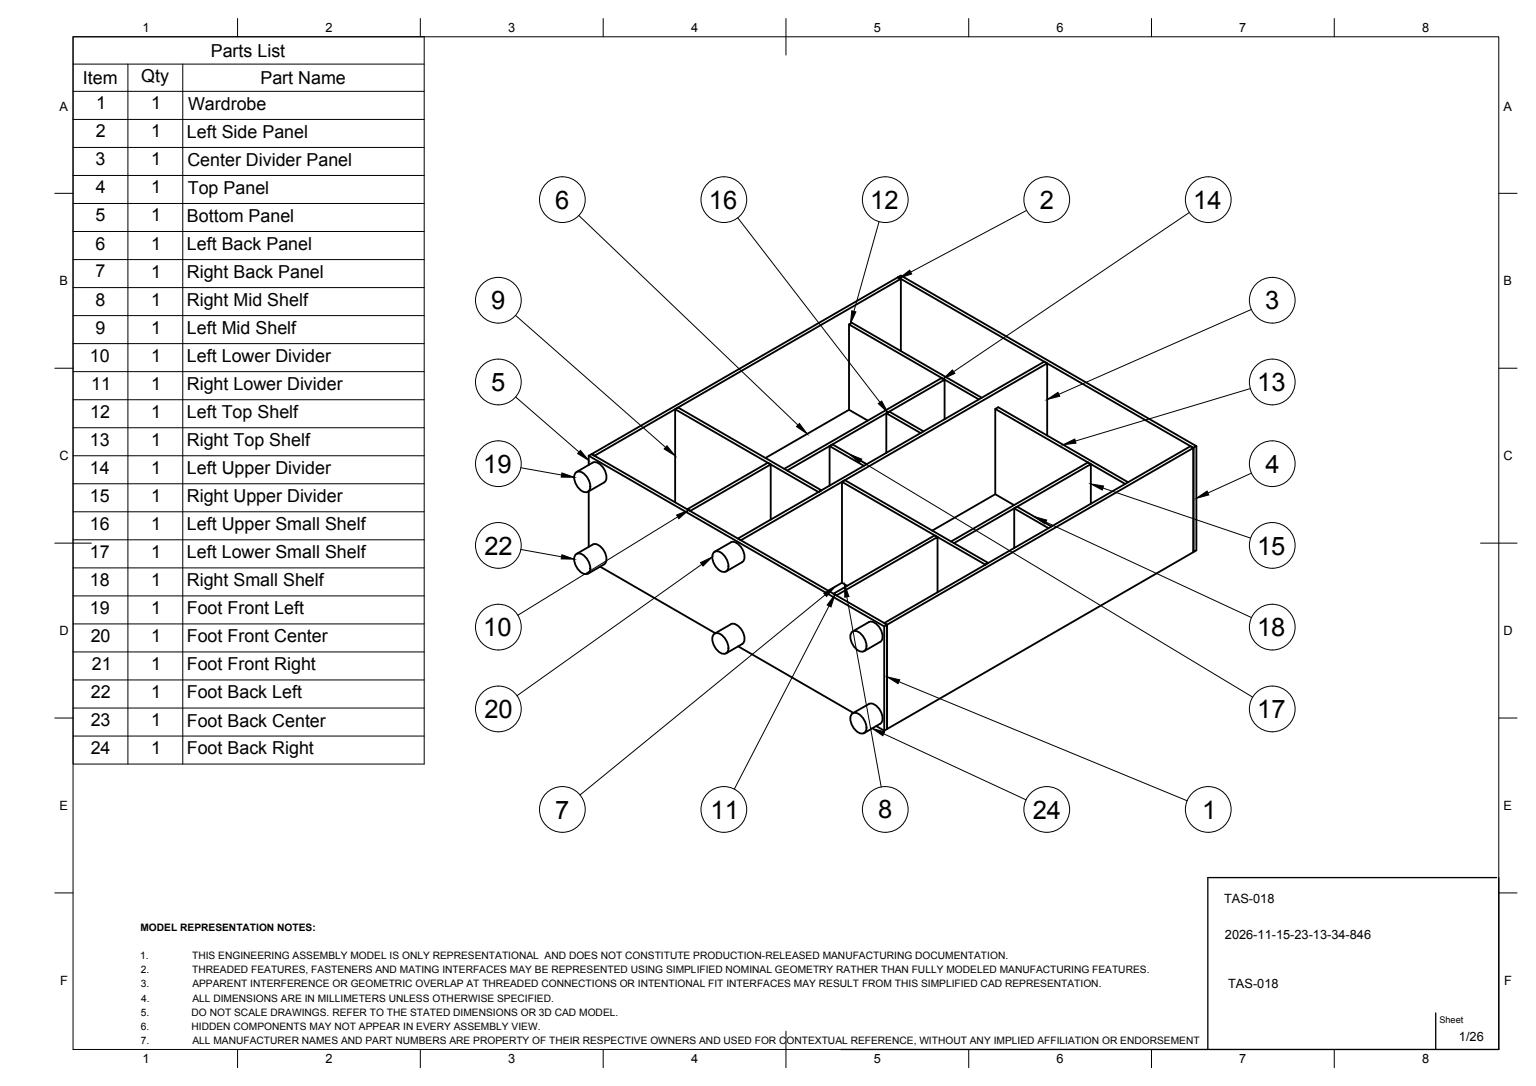
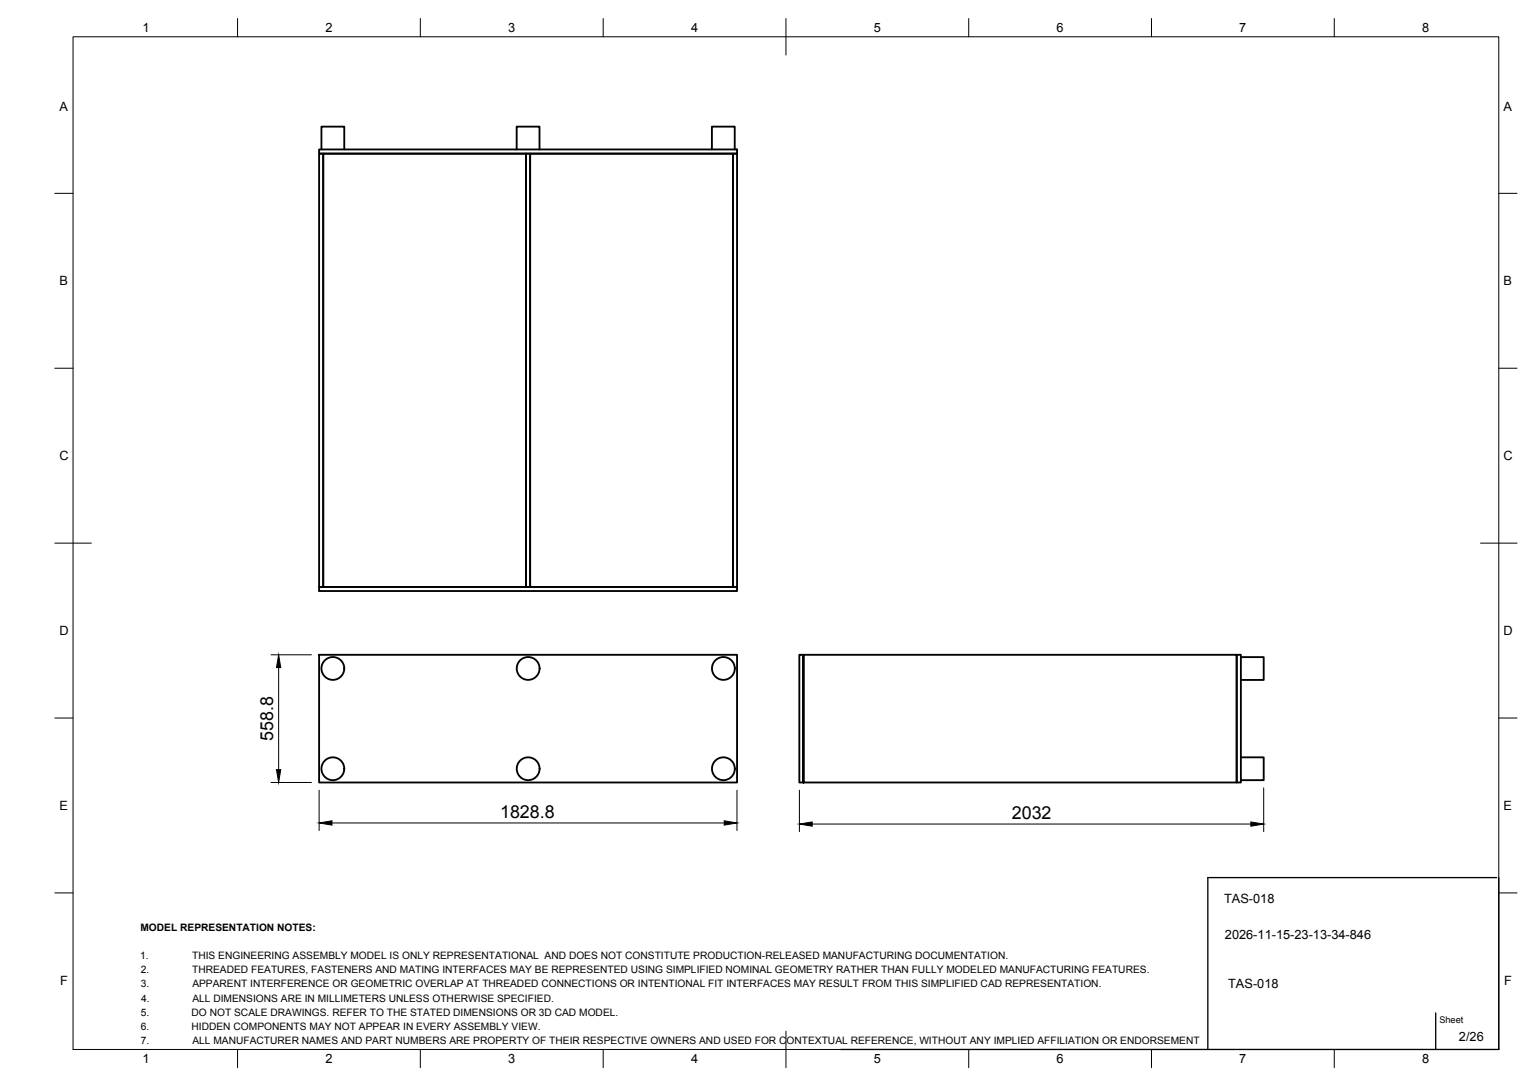
ISO-10303-21;
HEADER;
/* Generated by software containing ST-Developer
 * from STEP Tools, Inc. (www.steptools.com) 
 */

FILE_DESCRIPTION(
/* description */ (''),
/* implementation_level */ '2;1');

FILE_NAME(
/* name */ 'TAS-018.step',
/* time_stamp */ '2026-11-15T15:17:57-08:00',
/* author */ (''),
/* organization */ (''),
/* preprocessor_version */ 'ST-DEVELOPER v20.2',
/* originating_system */ 'Autodesk Translation Framework v15.17.0.0',
/* authorisation */ '');

FILE_SCHEMA (('AUTOMOTIVE_DESIGN { 1 0 10303 214 3 1 1 }'));
ENDSEC;

DATA;
#10=MECHANICAL_DESIGN_GEOMETRIC_PRESENTATION_REPRESENTATION('',(#177,#178,
#179,#180,#181,#182,#183,#184,#185,#186,#187,#188,#189,#190,#191,#192,#193,
#194,#195,#196,#197,#198,#199,#200),#3723);
#11=CIRCLE('',#2347,1.96850393700787);
#12=CIRCLE('',#2348,1.96850393700787);
#13=CIRCLE('',#2395,1.96850393700787);
#14=CIRCLE('',#2396,1.96850393700787);
#15=CIRCLE('',#2436,1.96850393700787);
#16=CIRCLE('',#2437,1.96850393700787);
#17=CIRCLE('',#2442,1.96850393700787);
#18=CIRCLE('',#2443,1.96850393700787);
#19=CIRCLE('',#2448,1.96850393700787);
#20=CIRCLE('',#2449,1.96850393700787);
#21=CIRCLE('',#2454,1.96850393700787);
#22=CIRCLE('',#2455,1.96850393700787);
#23=CYLINDRICAL_SURFACE('',#2346,1.96850393700787);
#24=CYLINDRICAL_SURFACE('',#2394,1.96850393700787);
#25=CYLINDRICAL_SURFACE('',#2435,1.96850393700787);
#26=CYLINDRICAL_SURFACE('',#2441,1.96850393700787);
#27=CYLINDRICAL_SURFACE('',#2447,1.96850393700787);
#28=CYLINDRICAL_SURFACE('',#2453,1.96850393700787);
#29=ITEM_DEFINED_TRANSFORMATION($,$,#2316,#2323);
#30=ITEM_DEFINED_TRANSFORMATION($,$,#2315,#2479);
#31=ITEM_DEFINED_TRANSFORMATION($,$,#2324,#2480);
#32=ITEM_DEFINED_TRANSFORMATION($,$,#2331,#2481);
#33=ITEM_DEFINED_TRANSFORMATION($,$,#2338,#2482);
#34=ITEM_DEFINED_TRANSFORMATION($,$,#2345,#2483);
#35=ITEM_DEFINED_TRANSFORMATION($,$,#2351,#2484);
#36=ITEM_DEFINED_TRANSFORMATION($,$,#2358,#2485);
#37=ITEM_DEFINED_TRANSFORMATION($,$,#2365,#2486);
#38=ITEM_DEFINED_TRANSFORMATION($,$,#2372,#2487);
#39=ITEM_DEFINED_TRANSFORMATION($,$,#2379,#2488);
#40=ITEM_DEFINED_TRANSFORMATION($,$,#2386,#2489);
#41=ITEM_DEFINED_TRANSFORMATION($,$,#2393,#2490);
#42=ITEM_DEFINED_TRANSFORMATION($,$,#2399,#2491);
#43=ITEM_DEFINED_TRANSFORMATION($,$,#2406,#2492);
#44=ITEM_DEFINED_TRANSFORMATION($,$,#2413,#2493);
#45=ITEM_DEFINED_TRANSFORMATION($,$,#2420,#2494);
#46=ITEM_DEFINED_TRANSFORMATION($,$,#2427,#2495);
#47=ITEM_DEFINED_TRANSFORMATION($,$,#2434,#2496);
#48=ITEM_DEFINED_TRANSFORMATION($,$,#2440,#2497);
#49=ITEM_DEFINED_TRANSFORMATION($,$,#2446,#2498);
#50=ITEM_DEFINED_TRANSFORMATION($,$,#2452,#2499);
#51=ITEM_DEFINED_TRANSFORMATION($,$,#2458,#2500);
#52=ITEM_DEFINED_TRANSFORMATION($,$,#2465,#2501);
#53=ITEM_DEFINED_TRANSFORMATION($,$,#2472,#2502);
#54=(
REPRESENTATION_RELATIONSHIP($,$,#3810,#3809)
REPRESENTATION_RELATIONSHIP_WITH_TRANSFORMATION(#29)
SHAPE_REPRESENTATION_RELATIONSHIP()
);
#55=(
REPRESENTATION_RELATIONSHIP($,$,#3809,#3808)
REPRESENTATION_RELATIONSHIP_WITH_TRANSFORMATION(#30)
SHAPE_REPRESENTATION_RELATIONSHIP()
);
#56=(
REPRESENTATION_RELATIONSHIP($,$,#3811,#3808)
REPRESENTATION_RELATIONSHIP_WITH_TRANSFORMATION(#31)
SHAPE_REPRESENTATION_RELATIONSHIP()
);
#57=(
REPRESENTATION_RELATIONSHIP($,$,#3812,#3808)
REPRESENTATION_RELATIONSHIP_WITH_TRANSFORMATION(#32)
SHAPE_REPRESENTATION_RELATIONSHIP()
);
#58=(
REPRESENTATION_RELATIONSHIP($,$,#3813,#3808)
REPRESENTATION_RELATIONSHIP_WITH_TRANSFORMATION(#33)
SHAPE_REPRESENTATION_RELATIONSHIP()
);
#59=(
REPRESENTATION_RELATIONSHIP($,$,#3814,#3808)
REPRESENTATION_RELATIONSHIP_WITH_TRANSFORMATION(#34)
SHAPE_REPRESENTATION_RELATIONSHIP()
);
#60=(
REPRESENTATION_RELATIONSHIP($,$,#3815,#3808)
REPRESENTATION_RELATIONSHIP_WITH_TRANSFORMATION(#35)
SHAPE_REPRESENTATION_RELATIONSHIP()
);
#61=(
REPRESENTATION_RELATIONSHIP($,$,#3816,#3808)
REPRESENTATION_RELATIONSHIP_WITH_TRANSFORMATION(#36)
SHAPE_REPRESENTATION_RELATIONSHIP()
);
#62=(
REPRESENTATION_RELATIONSHIP($,$,#3817,#3808)
REPRESENTATION_RELATIONSHIP_WITH_TRANSFORMATION(#37)
SHAPE_REPRESENTATION_RELATIONSHIP()
);
#63=(
REPRESENTATION_RELATIONSHIP($,$,#3818,#3808)
REPRESENTATION_RELATIONSHIP_WITH_TRANSFORMATION(#38)
SHAPE_REPRESENTATION_RELATIONSHIP()
);
#64=(
REPRESENTATION_RELATIONSHIP($,$,#3819,#3808)
REPRESENTATION_RELATIONSHIP_WITH_TRANSFORMATION(#39)
SHAPE_REPRESENTATION_RELATIONSHIP()
);
#65=(
REPRESENTATION_RELATIONSHIP($,$,#3820,#3808)
REPRESENTATION_RELATIONSHIP_WITH_TRANSFORMATION(#40)
SHAPE_REPRESENTATION_RELATIONSHIP()
);
#66=(
REPRESENTATION_RELATIONSHIP($,$,#3821,#3808)
REPRESENTATION_RELATIONSHIP_WITH_TRANSFORMATION(#41)
SHAPE_REPRESENTATION_RELATIONSHIP()
);
#67=(
REPRESENTATION_RELATIONSHIP($,$,#3822,#3808)
REPRESENTATION_RELATIONSHIP_WITH_TRANSFORMATION(#42)
SHAPE_REPRESENTATION_RELATIONSHIP()
);
#68=(
REPRESENTATION_RELATIONSHIP($,$,#3823,#3808)
REPRESENTATION_RELATIONSHIP_WITH_TRANSFORMATION(#43)
SHAPE_REPRESENTATION_RELATIONSHIP()
);
#69=(
REPRESENTATION_RELATIONSHIP($,$,#3824,#3808)
REPRESENTATION_RELATIONSHIP_WITH_TRANSFORMATION(#44)
SHAPE_REPRESENTATION_RELATIONSHIP()
);
#70=(
REPRESENTATION_RELATIONSHIP($,$,#3825,#3808)
REPRESENTATION_RELATIONSHIP_WITH_TRANSFORMATION(#45)
SHAPE_REPRESENTATION_RELATIONSHIP()
);
#71=(
REPRESENTATION_RELATIONSHIP($,$,#3826,#3808)
REPRESENTATION_RELATIONSHIP_WITH_TRANSFORMATION(#46)
SHAPE_REPRESENTATION_RELATIONSHIP()
);
#72=(
REPRESENTATION_RELATIONSHIP($,$,#3827,#3808)
REPRESENTATION_RELATIONSHIP_WITH_TRANSFORMATION(#47)
SHAPE_REPRESENTATION_RELATIONSHIP()
);
#73=(
REPRESENTATION_RELATIONSHIP($,$,#3828,#3808)
REPRESENTATION_RELATIONSHIP_WITH_TRANSFORMATION(#48)
SHAPE_REPRESENTATION_RELATIONSHIP()
);
#74=(
REPRESENTATION_RELATIONSHIP($,$,#3829,#3808)
REPRESENTATION_RELATIONSHIP_WITH_TRANSFORMATION(#49)
SHAPE_REPRESENTATION_RELATIONSHIP()
);
#75=(
REPRESENTATION_RELATIONSHIP($,$,#3830,#3808)
REPRESENTATION_RELATIONSHIP_WITH_TRANSFORMATION(#50)
SHAPE_REPRESENTATION_RELATIONSHIP()
);
#76=(
REPRESENTATION_RELATIONSHIP($,$,#3831,#3808)
REPRESENTATION_RELATIONSHIP_WITH_TRANSFORMATION(#51)
SHAPE_REPRESENTATION_RELATIONSHIP()
);
#77=(
REPRESENTATION_RELATIONSHIP($,$,#3832,#3808)
REPRESENTATION_RELATIONSHIP_WITH_TRANSFORMATION(#52)
SHAPE_REPRESENTATION_RELATIONSHIP()
);
#78=(
REPRESENTATION_RELATIONSHIP($,$,#3833,#3808)
REPRESENTATION_RELATIONSHIP_WITH_TRANSFORMATION(#53)
SHAPE_REPRESENTATION_RELATIONSHIP()
);
#79=CONTEXT_DEPENDENT_SHAPE_REPRESENTATION(#54,#3760);
#80=CONTEXT_DEPENDENT_SHAPE_REPRESENTATION(#55,#3784);
#81=CONTEXT_DEPENDENT_SHAPE_REPRESENTATION(#56,#3785);
#82=CONTEXT_DEPENDENT_SHAPE_REPRESENTATION(#57,#3786);
#83=CONTEXT_DEPENDENT_SHAPE_REPRESENTATION(#58,#3787);
#84=CONTEXT_DEPENDENT_SHAPE_REPRESENTATION(#59,#3788);
#85=CONTEXT_DEPENDENT_SHAPE_REPRESENTATION(#60,#3789);
#86=CONTEXT_DEPENDENT_SHAPE_REPRESENTATION(#61,#3790);
#87=CONTEXT_DEPENDENT_SHAPE_REPRESENTATION(#62,#3791);
#88=CONTEXT_DEPENDENT_SHAPE_REPRESENTATION(#63,#3792);
#89=CONTEXT_DEPENDENT_SHAPE_REPRESENTATION(#64,#3793);
#90=CONTEXT_DEPENDENT_SHAPE_REPRESENTATION(#65,#3794);
#91=CONTEXT_DEPENDENT_SHAPE_REPRESENTATION(#66,#3795);
#92=CONTEXT_DEPENDENT_SHAPE_REPRESENTATION(#67,#3796);
#93=CONTEXT_DEPENDENT_SHAPE_REPRESENTATION(#68,#3797);
#94=CONTEXT_DEPENDENT_SHAPE_REPRESENTATION(#69,#3798);
#95=CONTEXT_DEPENDENT_SHAPE_REPRESENTATION(#70,#3799);
#96=CONTEXT_DEPENDENT_SHAPE_REPRESENTATION(#71,#3800);
#97=CONTEXT_DEPENDENT_SHAPE_REPRESENTATION(#72,#3801);
#98=CONTEXT_DEPENDENT_SHAPE_REPRESENTATION(#73,#3802);
#99=CONTEXT_DEPENDENT_SHAPE_REPRESENTATION(#74,#3803);
#100=CONTEXT_DEPENDENT_SHAPE_REPRESENTATION(#75,#3804);
#101=CONTEXT_DEPENDENT_SHAPE_REPRESENTATION(#76,#3805);
#102=CONTEXT_DEPENDENT_SHAPE_REPRESENTATION(#77,#3806);
#103=CONTEXT_DEPENDENT_SHAPE_REPRESENTATION(#78,#3807);
#104=NEXT_ASSEMBLY_USAGE_OCCURRENCE('Right Side Panel:1',
'Right Side Panel:1','Right Side Panel:1',#3836,#3837,
'Right Side Panel:1');
#105=NEXT_ASSEMBLY_USAGE_OCCURRENCE('Wardrobe:1','Wardrobe:1',
'Wardrobe:1',#3835,#3836,'Wardrobe:1');
#106=NEXT_ASSEMBLY_USAGE_OCCURRENCE('Left Side Panel:1',
'Left Side Panel:1','Left Side Panel:1',#3835,#3838,'Left Side Panel:1');
#107=NEXT_ASSEMBLY_USAGE_OCCURRENCE('Center Divider Panel:1',
'Center Divider Panel:1','Center Divider Panel:1',#3835,#3839,
'Center Divider Panel:1');
#108=NEXT_ASSEMBLY_USAGE_OCCURRENCE('Left Lower Small Shelf:1',
'Left Lower Small Shelf:1','Left Lower Small Shelf:1',#3835,#3840,
'Left Lower Small Shelf:1');
#109=NEXT_ASSEMBLY_USAGE_OCCURRENCE('Foot Front Center:1',
'Foot Front Center:1','Foot Front Center:1',#3835,#3841,
'Foot Front Center:1');
#110=NEXT_ASSEMBLY_USAGE_OCCURRENCE('Left Lower Divider:1',
'Left Lower Divider:1','Left Lower Divider:1',#3835,#3842,
'Left Lower Divider:1');
#111=NEXT_ASSEMBLY_USAGE_OCCURRENCE('Right Top Shelf:1',
'Right Top Shelf:1','Right Top Shelf:1',#3835,#3843,'Right Top Shelf:1');
#112=NEXT_ASSEMBLY_USAGE_OCCURRENCE('Left Upper Small Shelf:1',
'Left Upper Small Shelf:1','Left Upper Small Shelf:1',#3835,#3844,
'Left Upper Small Shelf:1');
#113=NEXT_ASSEMBLY_USAGE_OCCURRENCE('Right Upper Divider:1',
'Right Upper Divider:1','Right Upper Divider:1',#3835,#3845,
'Right Upper Divider:1');
#114=NEXT_ASSEMBLY_USAGE_OCCURRENCE('Left Mid Shelf:1',
'Left Mid Shelf:1','Left Mid Shelf:1',#3835,#3846,'Left Mid Shelf:1');
#115=NEXT_ASSEMBLY_USAGE_OCCURRENCE('Right Lower Divider:1',
'Right Lower Divider:1','Right Lower Divider:1',#3835,#3847,
'Right Lower Divider:1');
#116=NEXT_ASSEMBLY_USAGE_OCCURRENCE('Foot Front Right:1',
'Foot Front Right:1','Foot Front Right:1',#3835,#3848,
'Foot Front Right:1');
#117=NEXT_ASSEMBLY_USAGE_OCCURRENCE('Right Mid Shelf:1',
'Right Mid Shelf:1','Right Mid Shelf:1',#3835,#3849,'Right Mid Shelf:1');
#118=NEXT_ASSEMBLY_USAGE_OCCURRENCE('Left Top Shelf:1',
'Left Top Shelf:1','Left Top Shelf:1',#3835,#3850,'Left Top Shelf:1');
#119=NEXT_ASSEMBLY_USAGE_OCCURRENCE('Right Small Shelf:1',
'Right Small Shelf:1','Right Small Shelf:1',#3835,#3851,
'Right Small Shelf:1');
#120=NEXT_ASSEMBLY_USAGE_OCCURRENCE('Left Upper Divider:1',
'Left Upper Divider:1','Left Upper Divider:1',#3835,#3852,
'Left Upper Divider:1');
#121=NEXT_ASSEMBLY_USAGE_OCCURRENCE('Top Panel:1','Top Panel:1',
'Top Panel:1',#3835,#3853,'Top Panel:1');
#122=NEXT_ASSEMBLY_USAGE_OCCURRENCE('Foot Front Left:1',
'Foot Front Left:1','Foot Front Left:1',#3835,#3854,'Foot Front Left:1');
#123=NEXT_ASSEMBLY_USAGE_OCCURRENCE('Foot Back Right:1',
'Foot Back Right:1','Foot Back Right:1',#3835,#3855,'Foot Back Right:1');
#124=NEXT_ASSEMBLY_USAGE_OCCURRENCE('Foot Back Left:1',
'Foot Back Left:1','Foot Back Left:1',#3835,#3856,'Foot Back Left:1');
#125=NEXT_ASSEMBLY_USAGE_OCCURRENCE('Foot Back Center:1',
'Foot Back Center:1','Foot Back Center:1',#3835,#3857,
'Foot Back Center:1');
#126=NEXT_ASSEMBLY_USAGE_OCCURRENCE('Left Back Panel:1',
'Left Back Panel:1','Left Back Panel:1',#3835,#3858,'Left Back Panel:1');
#127=NEXT_ASSEMBLY_USAGE_OCCURRENCE('Bottom Panel:1','Bottom Panel:1',
'Bottom Panel:1',#3835,#3859,'Bottom Panel:1');
#128=NEXT_ASSEMBLY_USAGE_OCCURRENCE('Right Back Panel:1',
'Right Back Panel:1','Right Back Panel:1',#3835,#3860,
'Right Back Panel:1');
#129=SHAPE_REPRESENTATION_RELATIONSHIP('SRR','None',#3810,#153);
#130=SHAPE_REPRESENTATION_RELATIONSHIP('SRR','None',#3811,#154);
#131=SHAPE_REPRESENTATION_RELATIONSHIP('SRR','None',#3812,#155);
#132=SHAPE_REPRESENTATION_RELATIONSHIP('SRR','None',#3813,#156);
#133=SHAPE_REPRESENTATION_RELATIONSHIP('SRR','None',#3814,#157);
#134=SHAPE_REPRESENTATION_RELATIONSHIP('SRR','None',#3815,#158);
#135=SHAPE_REPRESENTATION_RELATIONSHIP('SRR','None',#3816,#159);
#136=SHAPE_REPRESENTATION_RELATIONSHIP('SRR','None',#3817,#160);
#137=SHAPE_REPRESENTATION_RELATIONSHIP('SRR','None',#3818,#161);
#138=SHAPE_REPRESENTATION_RELATIONSHIP('SRR','None',#3819,#162);
#139=SHAPE_REPRESENTATION_RELATIONSHIP('SRR','None',#3820,#163);
#140=SHAPE_REPRESENTATION_RELATIONSHIP('SRR','None',#3821,#164);
#141=SHAPE_REPRESENTATION_RELATIONSHIP('SRR','None',#3822,#165);
#142=SHAPE_REPRESENTATION_RELATIONSHIP('SRR','None',#3823,#166);
#143=SHAPE_REPRESENTATION_RELATIONSHIP('SRR','None',#3824,#167);
#144=SHAPE_REPRESENTATION_RELATIONSHIP('SRR','None',#3825,#168);
#145=SHAPE_REPRESENTATION_RELATIONSHIP('SRR','None',#3826,#169);
#146=SHAPE_REPRESENTATION_RELATIONSHIP('SRR','None',#3827,#170);
#147=SHAPE_REPRESENTATION_RELATIONSHIP('SRR','None',#3828,#171);
#148=SHAPE_REPRESENTATION_RELATIONSHIP('SRR','None',#3829,#172);
#149=SHAPE_REPRESENTATION_RELATIONSHIP('SRR','None',#3830,#173);
#150=SHAPE_REPRESENTATION_RELATIONSHIP('SRR','None',#3831,#174);
#151=SHAPE_REPRESENTATION_RELATIONSHIP('SRR','None',#3832,#175);
#152=SHAPE_REPRESENTATION_RELATIONSHIP('SRR','None',#3833,#176);
#153=ADVANCED_BREP_SHAPE_REPRESENTATION('',(#201),#3699);
#154=ADVANCED_BREP_SHAPE_REPRESENTATION('',(#202),#3700);
#155=ADVANCED_BREP_SHAPE_REPRESENTATION('',(#203),#3701);
#156=ADVANCED_BREP_SHAPE_REPRESENTATION('',(#204),#3702);
#157=ADVANCED_BREP_SHAPE_REPRESENTATION('',(#205),#3703);
#158=ADVANCED_BREP_SHAPE_REPRESENTATION('',(#206),#3704);
#159=ADVANCED_BREP_SHAPE_REPRESENTATION('',(#207),#3705);
#160=ADVANCED_BREP_SHAPE_REPRESENTATION('',(#208),#3706);
#161=ADVANCED_BREP_SHAPE_REPRESENTATION('',(#209),#3707);
#162=ADVANCED_BREP_SHAPE_REPRESENTATION('',(#210),#3708);
#163=ADVANCED_BREP_SHAPE_REPRESENTATION('',(#211),#3709);
#164=ADVANCED_BREP_SHAPE_REPRESENTATION('',(#212),#3710);
#165=ADVANCED_BREP_SHAPE_REPRESENTATION('',(#213),#3711);
#166=ADVANCED_BREP_SHAPE_REPRESENTATION('',(#214),#3712);
#167=ADVANCED_BREP_SHAPE_REPRESENTATION('',(#215),#3713);
#168=ADVANCED_BREP_SHAPE_REPRESENTATION('',(#216),#3714);
#169=ADVANCED_BREP_SHAPE_REPRESENTATION('',(#217),#3715);
#170=ADVANCED_BREP_SHAPE_REPRESENTATION('',(#218),#3716);
#171=ADVANCED_BREP_SHAPE_REPRESENTATION('',(#219),#3717);
#172=ADVANCED_BREP_SHAPE_REPRESENTATION('',(#220),#3718);
#173=ADVANCED_BREP_SHAPE_REPRESENTATION('',(#221),#3719);
#174=ADVANCED_BREP_SHAPE_REPRESENTATION('',(#222),#3720);
#175=ADVANCED_BREP_SHAPE_REPRESENTATION('',(#223),#3721);
#176=ADVANCED_BREP_SHAPE_REPRESENTATION('',(#224),#3722);
#177=STYLED_ITEM('',(#3943),#201);
#178=STYLED_ITEM('',(#3943),#202);
#179=STYLED_ITEM('',(#3943),#203);
#180=STYLED_ITEM('',(#3944),#204);
#181=STYLED_ITEM('',(#3945),#205);
#182=STYLED_ITEM('',(#3946),#206);
#183=STYLED_ITEM('',(#3947),#207);
#184=STYLED_ITEM('',(#3944),#208);
#185=STYLED_ITEM('',(#3946),#209);
#186=STYLED_ITEM('',(#3947),#210);
#187=STYLED_ITEM('',(#3946),#211);
#188=STYLED_ITEM('',(#3945),#212);
#189=STYLED_ITEM('',(#3947),#213);
#190=STYLED_ITEM('',(#3947),#214);
#191=STYLED_ITEM('',(#3944),#215);
#192=STYLED_ITEM('',(#3946),#216);
#193=STYLED_ITEM('',(#3948),#217);
#194=STYLED_ITEM('',(#3945),#218);
#195=STYLED_ITEM('',(#3945),#219);
#196=STYLED_ITEM('',(#3945),#220);
#197=STYLED_ITEM('',(#3945),#221);
#198=STYLED_ITEM('',(#3949),#222);
#199=STYLED_ITEM('',(#3948),#223);
#200=STYLED_ITEM('',(#3949),#224);
#201=MANIFOLD_SOLID_BREP('Body1',#2025);
#202=MANIFOLD_SOLID_BREP('Body1',#2026);
#203=MANIFOLD_SOLID_BREP('Body1',#2027);
#204=MANIFOLD_SOLID_BREP('Body1',#2028);
#205=MANIFOLD_SOLID_BREP('Body1',#2029);
#206=MANIFOLD_SOLID_BREP('Body1',#2030);
#207=MANIFOLD_SOLID_BREP('Body1',#2031);
#208=MANIFOLD_SOLID_BREP('Body1',#2032);
#209=MANIFOLD_SOLID_BREP('Body1',#2033);
#210=MANIFOLD_SOLID_BREP('Body1',#2034);
#211=MANIFOLD_SOLID_BREP('Body1',#2035);
#212=MANIFOLD_SOLID_BREP('Body1',#2036);
#213=MANIFOLD_SOLID_BREP('Body1',#2037);
#214=MANIFOLD_SOLID_BREP('Body1',#2038);
#215=MANIFOLD_SOLID_BREP('Body1',#2039);
#216=MANIFOLD_SOLID_BREP('Body1',#2040);
#217=MANIFOLD_SOLID_BREP('Body1',#2041);
#218=MANIFOLD_SOLID_BREP('Body1',#2042);
#219=MANIFOLD_SOLID_BREP('Body1',#2043);
#220=MANIFOLD_SOLID_BREP('Body1',#2044);
#221=MANIFOLD_SOLID_BREP('Body1',#2045);
#222=MANIFOLD_SOLID_BREP('Body1',#2046);
#223=MANIFOLD_SOLID_BREP('Body1',#2047);
#224=MANIFOLD_SOLID_BREP('Body1',#2048);
#225=FACE_OUTER_BOUND('',#351,.T.);
#226=FACE_OUTER_BOUND('',#352,.T.);
#227=FACE_OUTER_BOUND('',#353,.T.);
#228=FACE_OUTER_BOUND('',#354,.T.);
#229=FACE_OUTER_BOUND('',#355,.T.);
#230=FACE_OUTER_BOUND('',#356,.T.);
#231=FACE_OUTER_BOUND('',#357,.T.);
#232=FACE_OUTER_BOUND('',#358,.T.);
#233=FACE_OUTER_BOUND('',#359,.T.);
#234=FACE_OUTER_BOUND('',#360,.T.);
#235=FACE_OUTER_BOUND('',#361,.T.);
#236=FACE_OUTER_BOUND('',#362,.T.);
#237=FACE_OUTER_BOUND('',#363,.T.);
#238=FACE_OUTER_BOUND('',#364,.T.);
#239=FACE_OUTER_BOUND('',#365,.T.);
#240=FACE_OUTER_BOUND('',#366,.T.);
#241=FACE_OUTER_BOUND('',#367,.T.);
#242=FACE_OUTER_BOUND('',#368,.T.);
#243=FACE_OUTER_BOUND('',#369,.T.);
#244=FACE_OUTER_BOUND('',#370,.T.);
#245=FACE_OUTER_BOUND('',#371,.T.);
#246=FACE_OUTER_BOUND('',#372,.T.);
#247=FACE_OUTER_BOUND('',#373,.T.);
#248=FACE_OUTER_BOUND('',#374,.T.);
#249=FACE_OUTER_BOUND('',#375,.T.);
#250=FACE_OUTER_BOUND('',#376,.T.);
#251=FACE_OUTER_BOUND('',#377,.T.);
#252=FACE_OUTER_BOUND('',#378,.T.);
#253=FACE_OUTER_BOUND('',#379,.T.);
#254=FACE_OUTER_BOUND('',#380,.T.);
#255=FACE_OUTER_BOUND('',#381,.T.);
#256=FACE_OUTER_BOUND('',#382,.T.);
#257=FACE_OUTER_BOUND('',#383,.T.);
#258=FACE_OUTER_BOUND('',#384,.T.);
#259=FACE_OUTER_BOUND('',#385,.T.);
#260=FACE_OUTER_BOUND('',#386,.T.);
#261=FACE_OUTER_BOUND('',#387,.T.);
#262=FACE_OUTER_BOUND('',#388,.T.);
#263=FACE_OUTER_BOUND('',#389,.T.);
#264=FACE_OUTER_BOUND('',#390,.T.);
#265=FACE_OUTER_BOUND('',#391,.T.);
#266=FACE_OUTER_BOUND('',#392,.T.);
#267=FACE_OUTER_BOUND('',#393,.T.);
#268=FACE_OUTER_BOUND('',#394,.T.);
#269=FACE_OUTER_BOUND('',#395,.T.);
#270=FACE_OUTER_BOUND('',#396,.T.);
#271=FACE_OUTER_BOUND('',#397,.T.);
#272=FACE_OUTER_BOUND('',#398,.T.);
#273=FACE_OUTER_BOUND('',#399,.T.);
#274=FACE_OUTER_BOUND('',#400,.T.);
#275=FACE_OUTER_BOUND('',#401,.T.);
#276=FACE_OUTER_BOUND('',#402,.T.);
#277=FACE_OUTER_BOUND('',#403,.T.);
#278=FACE_OUTER_BOUND('',#404,.T.);
#279=FACE_OUTER_BOUND('',#405,.T.);
#280=FACE_OUTER_BOUND('',#406,.T.);
#281=FACE_OUTER_BOUND('',#407,.T.);
#282=FACE_OUTER_BOUND('',#408,.T.);
#283=FACE_OUTER_BOUND('',#409,.T.);
#284=FACE_OUTER_BOUND('',#410,.T.);
#285=FACE_OUTER_BOUND('',#411,.T.);
#286=FACE_OUTER_BOUND('',#412,.T.);
#287=FACE_OUTER_BOUND('',#413,.T.);
#288=FACE_OUTER_BOUND('',#414,.T.);
#289=FACE_OUTER_BOUND('',#415,.T.);
#290=FACE_OUTER_BOUND('',#416,.T.);
#291=FACE_OUTER_BOUND('',#417,.T.);
#292=FACE_OUTER_BOUND('',#418,.T.);
#293=FACE_OUTER_BOUND('',#419,.T.);
#294=FACE_OUTER_BOUND('',#420,.T.);
#295=FACE_OUTER_BOUND('',#421,.T.);
#296=FACE_OUTER_BOUND('',#422,.T.);
#297=FACE_OUTER_BOUND('',#423,.T.);
#298=FACE_OUTER_BOUND('',#424,.T.);
#299=FACE_OUTER_BOUND('',#425,.T.);
#300=FACE_OUTER_BOUND('',#426,.T.);
#301=FACE_OUTER_BOUND('',#427,.T.);
#302=FACE_OUTER_BOUND('',#428,.T.);
#303=FACE_OUTER_BOUND('',#429,.T.);
#304=FACE_OUTER_BOUND('',#430,.T.);
#305=FACE_OUTER_BOUND('',#431,.T.);
#306=FACE_OUTER_BOUND('',#432,.T.);
#307=FACE_OUTER_BOUND('',#433,.T.);
#308=FACE_OUTER_BOUND('',#434,.T.);
#309=FACE_OUTER_BOUND('',#435,.T.);
#310=FACE_OUTER_BOUND('',#436,.T.);
#311=FACE_OUTER_BOUND('',#437,.T.);
#312=FACE_OUTER_BOUND('',#438,.T.);
#313=FACE_OUTER_BOUND('',#439,.T.);
#314=FACE_OUTER_BOUND('',#440,.T.);
#315=FACE_OUTER_BOUND('',#441,.T.);
#316=FACE_OUTER_BOUND('',#442,.T.);
#317=FACE_OUTER_BOUND('',#443,.T.);
#318=FACE_OUTER_BOUND('',#444,.T.);
#319=FACE_OUTER_BOUND('',#445,.T.);
#320=FACE_OUTER_BOUND('',#446,.T.);
#321=FACE_OUTER_BOUND('',#447,.T.);
#322=FACE_OUTER_BOUND('',#448,.T.);
#323=FACE_OUTER_BOUND('',#449,.T.);
#324=FACE_OUTER_BOUND('',#450,.T.);
#325=FACE_OUTER_BOUND('',#451,.T.);
#326=FACE_OUTER_BOUND('',#452,.T.);
#327=FACE_OUTER_BOUND('',#453,.T.);
#328=FACE_OUTER_BOUND('',#454,.T.);
#329=FACE_OUTER_BOUND('',#455,.T.);
#330=FACE_OUTER_BOUND('',#456,.T.);
#331=FACE_OUTER_BOUND('',#457,.T.);
#332=FACE_OUTER_BOUND('',#458,.T.);
#333=FACE_OUTER_BOUND('',#459,.T.);
#334=FACE_OUTER_BOUND('',#460,.T.);
#335=FACE_OUTER_BOUND('',#461,.T.);
#336=FACE_OUTER_BOUND('',#462,.T.);
#337=FACE_OUTER_BOUND('',#463,.T.);
#338=FACE_OUTER_BOUND('',#464,.T.);
#339=FACE_OUTER_BOUND('',#465,.T.);
#340=FACE_OUTER_BOUND('',#466,.T.);
#341=FACE_OUTER_BOUND('',#467,.T.);
#342=FACE_OUTER_BOUND('',#468,.T.);
#343=FACE_OUTER_BOUND('',#469,.T.);
#344=FACE_OUTER_BOUND('',#470,.T.);
#345=FACE_OUTER_BOUND('',#471,.T.);
#346=FACE_OUTER_BOUND('',#472,.T.);
#347=FACE_OUTER_BOUND('',#473,.T.);
#348=FACE_OUTER_BOUND('',#474,.T.);
#349=FACE_OUTER_BOUND('',#475,.T.);
#350=FACE_OUTER_BOUND('',#476,.T.);
#351=EDGE_LOOP('',(#1311,#1312,#1313,#1314));
#352=EDGE_LOOP('',(#1315,#1316,#1317,#1318));
#353=EDGE_LOOP('',(#1319,#1320,#1321,#1322));
#354=EDGE_LOOP('',(#1323,#1324,#1325,#1326));
#355=EDGE_LOOP('',(#1327,#1328,#1329,#1330));
#356=EDGE_LOOP('',(#1331,#1332,#1333,#1334));
#357=EDGE_LOOP('',(#1335,#1336,#1337,#1338));
#358=EDGE_LOOP('',(#1339,#1340,#1341,#1342));
#359=EDGE_LOOP('',(#1343,#1344,#1345,#1346));
#360=EDGE_LOOP('',(#1347,#1348,#1349,#1350));
#361=EDGE_LOOP('',(#1351,#1352,#1353,#1354));
#362=EDGE_LOOP('',(#1355,#1356,#1357,#1358));
#363=EDGE_LOOP('',(#1359,#1360,#1361,#1362));
#364=EDGE_LOOP('',(#1363,#1364,#1365,#1366));
#365=EDGE_LOOP('',(#1367,#1368,#1369,#1370));
#366=EDGE_LOOP('',(#1371,#1372,#1373,#1374));
#367=EDGE_LOOP('',(#1375,#1376,#1377,#1378));
#368=EDGE_LOOP('',(#1379,#1380,#1381,#1382));
#369=EDGE_LOOP('',(#1383,#1384,#1385,#1386));
#370=EDGE_LOOP('',(#1387,#1388,#1389,#1390));
#371=EDGE_LOOP('',(#1391,#1392,#1393,#1394));
#372=EDGE_LOOP('',(#1395,#1396,#1397,#1398));
#373=EDGE_LOOP('',(#1399,#1400,#1401,#1402));
#374=EDGE_LOOP('',(#1403,#1404,#1405,#1406));
#375=EDGE_LOOP('',(#1407,#1408,#1409,#1410));
#376=EDGE_LOOP('',(#1411));
#377=EDGE_LOOP('',(#1412));
#378=EDGE_LOOP('',(#1413,#1414,#1415,#1416));
#379=EDGE_LOOP('',(#1417,#1418,#1419,#1420));
#380=EDGE_LOOP('',(#1421,#1422,#1423,#1424));
#381=EDGE_LOOP('',(#1425,#1426,#1427,#1428));
#382=EDGE_LOOP('',(#1429,#1430,#1431,#1432));
#383=EDGE_LOOP('',(#1433,#1434,#1435,#1436));
#384=EDGE_LOOP('',(#1437,#1438,#1439,#1440));
#385=EDGE_LOOP('',(#1441,#1442,#1443,#1444));
#386=EDGE_LOOP('',(#1445,#1446,#1447,#1448));
#387=EDGE_LOOP('',(#1449,#1450,#1451,#1452));
#388=EDGE_LOOP('',(#1453,#1454,#1455,#1456));
#389=EDGE_LOOP('',(#1457,#1458,#1459,#1460));
#390=EDGE_LOOP('',(#1461,#1462,#1463,#1464));
#391=EDGE_LOOP('',(#1465,#1466,#1467,#1468));
#392=EDGE_LOOP('',(#1469,#1470,#1471,#1472));
#393=EDGE_LOOP('',(#1473,#1474,#1475,#1476));
#394=EDGE_LOOP('',(#1477,#1478,#1479,#1480));
#395=EDGE_LOOP('',(#1481,#1482,#1483,#1484));
#396=EDGE_LOOP('',(#1485,#1486,#1487,#1488));
#397=EDGE_LOOP('',(#1489,#1490,#1491,#1492));
#398=EDGE_LOOP('',(#1493,#1494,#1495,#1496));
#399=EDGE_LOOP('',(#1497,#1498,#1499,#1500));
#400=EDGE_LOOP('',(#1501,#1502,#1503,#1504));
#401=EDGE_LOOP('',(#1505,#1506,#1507,#1508));
#402=EDGE_LOOP('',(#1509,#1510,#1511,#1512));
#403=EDGE_LOOP('',(#1513,#1514,#1515,#1516));
#404=EDGE_LOOP('',(#1517,#1518,#1519,#1520));
#405=EDGE_LOOP('',(#1521,#1522,#1523,#1524));
#406=EDGE_LOOP('',(#1525,#1526,#1527,#1528));
#407=EDGE_LOOP('',(#1529,#1530,#1531,#1532));
#408=EDGE_LOOP('',(#1533,#1534,#1535,#1536));
#409=EDGE_LOOP('',(#1537,#1538,#1539,#1540));
#410=EDGE_LOOP('',(#1541,#1542,#1543,#1544));
#411=EDGE_LOOP('',(#1545,#1546,#1547,#1548));
#412=EDGE_LOOP('',(#1549,#1550,#1551,#1552));
#413=EDGE_LOOP('',(#1553,#1554,#1555,#1556));
#414=EDGE_LOOP('',(#1557,#1558,#1559,#1560));
#415=EDGE_LOOP('',(#1561));
#416=EDGE_LOOP('',(#1562));
#417=EDGE_LOOP('',(#1563,#1564,#1565,#1566));
#418=EDGE_LOOP('',(#1567,#1568,#1569,#1570));
#419=EDGE_LOOP('',(#1571,#1572,#1573,#1574));
#420=EDGE_LOOP('',(#1575,#1576,#1577,#1578));
#421=EDGE_LOOP('',(#1579,#1580,#1581,#1582));
#422=EDGE_LOOP('',(#1583,#1584,#1585,#1586));
#423=EDGE_LOOP('',(#1587,#1588,#1589,#1590));
#424=EDGE_LOOP('',(#1591,#1592,#1593,#1594));
#425=EDGE_LOOP('',(#1595,#1596,#1597,#1598));
#426=EDGE_LOOP('',(#1599,#1600,#1601,#1602));
#427=EDGE_LOOP('',(#1603,#1604,#1605,#1606));
#428=EDGE_LOOP('',(#1607,#1608,#1609,#1610));
#429=EDGE_LOOP('',(#1611,#1612,#1613,#1614));
#430=EDGE_LOOP('',(#1615,#1616,#1617,#1618));
#431=EDGE_LOOP('',(#1619,#1620,#1621,#1622));
#432=EDGE_LOOP('',(#1623,#1624,#1625,#1626));
#433=EDGE_LOOP('',(#1627,#1628,#1629,#1630));
#434=EDGE_LOOP('',(#1631,#1632,#1633,#1634));
#435=EDGE_LOOP('',(#1635,#1636,#1637,#1638));
#436=EDGE_LOOP('',(#1639,#1640,#1641,#1642));
#437=EDGE_LOOP('',(#1643,#1644,#1645,#1646));
#438=EDGE_LOOP('',(#1647,#1648,#1649,#1650));
#439=EDGE_LOOP('',(#1651,#1652,#1653,#1654));
#440=EDGE_LOOP('',(#1655,#1656,#1657,#1658));
#441=EDGE_LOOP('',(#1659,#1660,#1661,#1662));
#442=EDGE_LOOP('',(#1663,#1664,#1665,#1666));
#443=EDGE_LOOP('',(#1667,#1668,#1669,#1670));
#444=EDGE_LOOP('',(#1671,#1672,#1673,#1674));
#445=EDGE_LOOP('',(#1675,#1676,#1677,#1678));
#446=EDGE_LOOP('',(#1679,#1680,#1681,#1682));
#447=EDGE_LOOP('',(#1683,#1684,#1685,#1686));
#448=EDGE_LOOP('',(#1687));
#449=EDGE_LOOP('',(#1688));
#450=EDGE_LOOP('',(#1689,#1690,#1691,#1692));
#451=EDGE_LOOP('',(#1693));
#452=EDGE_LOOP('',(#1694));
#453=EDGE_LOOP('',(#1695,#1696,#1697,#1698));
#454=EDGE_LOOP('',(#1699));
#455=EDGE_LOOP('',(#1700));
#456=EDGE_LOOP('',(#1701,#1702,#1703,#1704));
#457=EDGE_LOOP('',(#1705));
#458=EDGE_LOOP('',(#1706));
#459=EDGE_LOOP('',(#1707,#1708,#1709,#1710));
#460=EDGE_LOOP('',(#1711,#1712,#1713,#1714));
#461=EDGE_LOOP('',(#1715,#1716,#1717,#1718));
#462=EDGE_LOOP('',(#1719,#1720,#1721,#1722));
#463=EDGE_LOOP('',(#1723,#1724,#1725,#1726));
#464=EDGE_LOOP('',(#1727,#1728,#1729,#1730));
#465=EDGE_LOOP('',(#1731,#1732,#1733,#1734));
#466=EDGE_LOOP('',(#1735,#1736,#1737,#1738));
#467=EDGE_LOOP('',(#1739,#1740,#1741,#1742));
#468=EDGE_LOOP('',(#1743,#1744,#1745,#1746));
#469=EDGE_LOOP('',(#1747,#1748,#1749,#1750));
#470=EDGE_LOOP('',(#1751,#1752,#1753,#1754));
#471=EDGE_LOOP('',(#1755,#1756,#1757,#1758));
#472=EDGE_LOOP('',(#1759,#1760,#1761,#1762));
#473=EDGE_LOOP('',(#1763,#1764,#1765,#1766));
#474=EDGE_LOOP('',(#1767,#1768,#1769,#1770));
#475=EDGE_LOOP('',(#1771,#1772,#1773,#1774));
#476=EDGE_LOOP('',(#1775,#1776,#1777,#1778));
#477=LINE('',#3109,#699);
#478=LINE('',#3111,#700);
#479=LINE('',#3113,#701);
#480=LINE('',#3114,#702);
#481=LINE('',#3117,#703);
#482=LINE('',#3119,#704);
#483=LINE('',#3120,#705);
#484=LINE('',#3123,#706);
#485=LINE('',#3125,#707);
#486=LINE('',#3126,#708);
#487=LINE('',#3128,#709);
#488=LINE('',#3129,#710);
#489=LINE('',#3137,#711);
#490=LINE('',#3139,#712);
#491=LINE('',#3141,#713);
#492=LINE('',#3142,#714);
#493=LINE('',#3145,#715);
#494=LINE('',#3147,#716);
#495=LINE('',#3148,#717);
#496=LINE('',#3151,#718);
#497=LINE('',#3153,#719);
#498=LINE('',#3154,#720);
#499=LINE('',#3156,#721);
#500=LINE('',#3157,#722);
#501=LINE('',#3164,#723);
#502=LINE('',#3166,#724);
#503=LINE('',#3168,#725);
#504=LINE('',#3169,#726);
#505=LINE('',#3172,#727);
#506=LINE('',#3174,#728);
#507=LINE('',#3175,#729);
#508=LINE('',#3178,#730);
#509=LINE('',#3180,#731);
#510=LINE('',#3181,#732);
#511=LINE('',#3183,#733);
#512=LINE('',#3184,#734);
#513=LINE('',#3191,#735);
#514=LINE('',#3193,#736);
#515=LINE('',#3195,#737);
#516=LINE('',#3196,#738);
#517=LINE('',#3199,#739);
#518=LINE('',#3201,#740);
#519=LINE('',#3202,#741);
#520=LINE('',#3205,#742);
#521=LINE('',#3207,#743);
#522=LINE('',#3208,#744);
#523=LINE('',#3210,#745);
#524=LINE('',#3211,#746);
#525=LINE('',#3219,#747);
#526=LINE('',#3227,#748);
#527=LINE('',#3229,#749);
#528=LINE('',#3231,#750);
#529=LINE('',#3232,#751);
#530=LINE('',#3235,#752);
#531=LINE('',#3237,#753);
#532=LINE('',#3238,#754);
#533=LINE('',#3241,#755);
#534=LINE('',#3243,#756);
#535=LINE('',#3244,#757);
#536=LINE('',#3246,#758);
#537=LINE('',#3247,#759);
#538=LINE('',#3254,#760);
#539=LINE('',#3256,#761);
#540=LINE('',#3258,#762);
#541=LINE('',#3259,#763);
#542=LINE('',#3262,#764);
#543=LINE('',#3264,#765);
#544=LINE('',#3265,#766);
#545=LINE('',#3268,#767);
#546=LINE('',#3270,#768);
#547=LINE('',#3271,#769);
#548=LINE('',#3273,#770);
#549=LINE('',#3274,#771);
#550=LINE('',#3281,#772);
#551=LINE('',#3283,#773);
#552=LINE('',#3285,#774);
#553=LINE('',#3286,#775);
#554=LINE('',#3289,#776);
#555=LINE('',#3291,#777);
#556=LINE('',#3292,#778);
#557=LINE('',#3295,#779);
#558=LINE('',#3297,#780);
#559=LINE('',#3298,#781);
#560=LINE('',#3300,#782);
#561=LINE('',#3301,#783);
#562=LINE('',#3308,#784);
#563=LINE('',#3310,#785);
#564=LINE('',#3312,#786);
#565=LINE('',#3313,#787);
#566=LINE('',#3316,#788);
#567=LINE('',#3318,#789);
#568=LINE('',#3319,#790);
#569=LINE('',#3322,#791);
#570=LINE('',#3324,#792);
#571=LINE('',#3325,#793);
#572=LINE('',#3327,#794);
#573=LINE('',#3328,#795);
#574=LINE('',#3335,#796);
#575=LINE('',#3337,#797);
#576=LINE('',#3339,#798);
#577=LINE('',#3340,#799);
#578=LINE('',#3344,#800);
#579=LINE('',#3346,#801);
#580=LINE('',#3348,#802);
#581=LINE('',#3349,#803);
#582=LINE('',#3351,#804);
#583=LINE('',#3352,#805);
#584=LINE('',#3354,#806);
#585=LINE('',#3356,#807);
#586=LINE('',#3362,#808);
#587=LINE('',#3364,#809);
#588=LINE('',#3366,#810);
#589=LINE('',#3367,#811);
#590=LINE('',#3371,#812);
#591=LINE('',#3372,#813);
#592=LINE('',#3373,#814);
#593=LINE('',#3376,#815);
#594=LINE('',#3378,#816);
#595=LINE('',#3379,#817);
#596=LINE('',#3381,#818);
#597=LINE('',#3382,#819);
#598=LINE('',#3390,#820);
#599=LINE('',#3398,#821);
#600=LINE('',#3400,#822);
#601=LINE('',#3402,#823);
#602=LINE('',#3403,#824);
#603=LINE('',#3407,#825);
#604=LINE('',#3409,#826);
#605=LINE('',#3411,#827);
#606=LINE('',#3412,#828);
#607=LINE('',#3414,#829);
#608=LINE('',#3415,#830);
#609=LINE('',#3417,#831);
#610=LINE('',#3419,#832);
#611=LINE('',#3425,#833);
#612=LINE('',#3427,#834);
#613=LINE('',#3429,#835);
#614=LINE('',#3430,#836);
#615=LINE('',#3433,#837);
#616=LINE('',#3435,#838);
#617=LINE('',#3436,#839);
#618=LINE('',#3439,#840);
#619=LINE('',#3441,#841);
#620=LINE('',#3442,#842);
#621=LINE('',#3444,#843);
#622=LINE('',#3445,#844);
#623=LINE('',#3452,#845);
#624=LINE('',#3454,#846);
#625=LINE('',#3456,#847);
#626=LINE('',#3457,#848);
#627=LINE('',#3460,#849);
#628=LINE('',#3462,#850);
#629=LINE('',#3463,#851);
#630=LINE('',#3466,#852);
#631=LINE('',#3468,#853);
#632=LINE('',#3469,#854);
#633=LINE('',#3471,#855);
#634=LINE('',#3472,#856);
#635=LINE('',#3479,#857);
#636=LINE('',#3481,#858);
#637=LINE('',#3483,#859);
#638=LINE('',#3484,#860);
#639=LINE('',#3487,#861);
#640=LINE('',#3489,#862);
#641=LINE('',#3490,#863);
#642=LINE('',#3493,#864);
#643=LINE('',#3495,#865);
#644=LINE('',#3496,#866);
#645=LINE('',#3498,#867);
#646=LINE('',#3499,#868);
#647=LINE('',#3506,#869);
#648=LINE('',#3508,#870);
#649=LINE('',#3510,#871);
#650=LINE('',#3511,#872);
#651=LINE('',#3514,#873);
#652=LINE('',#3516,#874);
#653=LINE('',#3517,#875);
#654=LINE('',#3520,#876);
#655=LINE('',#3522,#877);
#656=LINE('',#3523,#878);
#657=LINE('',#3525,#879);
#658=LINE('',#3526,#880);
#659=LINE('',#3534,#881);
#660=LINE('',#3543,#882);
#661=LINE('',#3552,#883);
#662=LINE('',#3561,#884);
#663=LINE('',#3569,#885);
#664=LINE('',#3571,#886);
#665=LINE('',#3573,#887);
#666=LINE('',#3574,#888);
#667=LINE('',#3577,#889);
#668=LINE('',#3579,#890);
#669=LINE('',#3580,#891);
#670=LINE('',#3583,#892);
#671=LINE('',#3585,#893);
#672=LINE('',#3586,#894);
#673=LINE('',#3588,#895);
#674=LINE('',#3589,#896);
#675=LINE('',#3596,#897);
#676=LINE('',#3598,#898);
#677=LINE('',#3600,#899);
#678=LINE('',#3601,#900);
#679=LINE('',#3604,#901);
#680=LINE('',#3606,#902);
#681=LINE('',#3607,#903);
#682=LINE('',#3610,#904);
#683=LINE('',#3612,#905);
#684=LINE('',#3613,#906);
#685=LINE('',#3615,#907);
#686=LINE('',#3616,#908);
#687=LINE('',#3623,#909);
#688=LINE('',#3625,#910);
#689=LINE('',#3627,#911);
#690=LINE('',#3628,#912);
#691=LINE('',#3631,#913);
#692=LINE('',#3633,#914);
#693=LINE('',#3634,#915);
#694=LINE('',#3637,#916);
#695=LINE('',#3639,#917);
#696=LINE('',#3640,#918);
#697=LINE('',#3642,#919);
#698=LINE('',#3643,#920);
#699=VECTOR('',#2511,74.6456692913386);
#700=VECTOR('',#2512,22.);
#701=VECTOR('',#2513,74.6456692913386);
#702=VECTOR('',#2514,22.);
#703=VECTOR('',#2517,0.708661417322833);
#704=VECTOR('',#2518,22.);
#705=VECTOR('',#2519,0.708661417322833);
#706=VECTOR('',#2522,74.6456692913386);
#707=VECTOR('',#2523,22.);
#708=VECTOR('',#2524,74.6456692913386);
#709=VECTOR('',#2527,0.708661417322833);
#710=VECTOR('',#2528,0.708661417322833);
#711=VECTOR('',#2539,74.6456692913386);
#712=VECTOR('',#2540,22.);
#713=VECTOR('',#2541,74.6456692913386);
#714=VECTOR('',#2542,22.);
#715=VECTOR('',#2545,0.708661417322833);
#716=VECTOR('',#2546,22.);
#717=VECTOR('',#2547,0.708661417322833);
#718=VECTOR('',#2550,74.6456692913386);
#719=VECTOR('',#2551,22.);
#720=VECTOR('',#2552,74.6456692913386);
#721=VECTOR('',#2555,0.708661417322833);
#722=VECTOR('',#2556,0.708661417322833);
#723=VECTOR('',#2565,74.6456692913386);
#724=VECTOR('',#2566,22.);
#725=VECTOR('',#2567,74.6456692913386);
#726=VECTOR('',#2568,22.);
#727=VECTOR('',#2571,0.708661417322835);
#728=VECTOR('',#2572,22.);
#729=VECTOR('',#2573,0.708661417322835);
#730=VECTOR('',#2576,74.6456692913386);
#731=VECTOR('',#2577,22.);
#732=VECTOR('',#2578,74.6456692913386);
#733=VECTOR('',#2581,0.708661417322835);
#734=VECTOR('',#2582,0.708661417322835);
#735=VECTOR('',#2591,0.708661417322833);
#736=VECTOR('',#2592,18.);
#737=VECTOR('',#2593,0.708661417322833);
#738=VECTOR('',#2594,18.);
#739=VECTOR('',#2597,11.6456692913385);
#740=VECTOR('',#2598,11.6456692913385);
#741=VECTOR('',#2599,18.);
#742=VECTOR('',#2602,0.708661417322833);
#743=VECTOR('',#2603,0.708661417322833);
#744=VECTOR('',#2604,18.);
#745=VECTOR('',#2607,11.6456692913385);
#746=VECTOR('',#2608,11.6456692913385);
#747=VECTOR('',#2619,1.96850393700787);
#748=VECTOR('',#2630,21.2913385826772);
#749=VECTOR('',#2631,19.6456692913386);
#750=VECTOR('',#2632,21.2913385826772);
#751=VECTOR('',#2633,19.6456692913386);
#752=VECTOR('',#2636,0.708661417322832);
#753=VECTOR('',#2637,0.708661417322832);
#754=VECTOR('',#2638,21.2913385826772);
#755=VECTOR('',#2641,19.6456692913386);
#756=VECTOR('',#2642,19.6456692913386);
#757=VECTOR('',#2643,21.2913385826772);
#758=VECTOR('',#2646,0.708661417322832);
#759=VECTOR('',#2647,0.708661417322832);
#760=VECTOR('',#2656,0.708661417322839);
#761=VECTOR('',#2657,18.);
#762=VECTOR('',#2658,0.708661417322839);
#763=VECTOR('',#2659,18.);
#764=VECTOR('',#2662,34.9370078740157);
#765=VECTOR('',#2663,18.);
#766=VECTOR('',#2664,34.9370078740157);
#767=VECTOR('',#2667,0.708661417322839);
#768=VECTOR('',#2668,18.);
#769=VECTOR('',#2669,0.708661417322839);
#770=VECTOR('',#2672,34.9370078740157);
#771=VECTOR('',#2673,34.9370078740157);
#772=VECTOR('',#2682,0.708661417322828);
#773=VECTOR('',#2683,18.);
#774=VECTOR('',#2684,0.708661417322828);
#775=VECTOR('',#2685,18.);
#776=VECTOR('',#2688,11.6456692913386);
#777=VECTOR('',#2689,11.6456692913386);
#778=VECTOR('',#2690,18.);
#779=VECTOR('',#2693,0.708661417322839);
#780=VECTOR('',#2694,0.708661417322839);
#781=VECTOR('',#2695,18.);
#782=VECTOR('',#2698,11.6456692913386);
#783=VECTOR('',#2699,11.6456692913386);
#784=VECTOR('',#2708,36.6456692913386);
#785=VECTOR('',#2709,18.);
#786=VECTOR('',#2710,36.6456692913386);
#787=VECTOR('',#2711,18.);
#788=VECTOR('',#2714,0.708661417322839);
#789=VECTOR('',#2715,0.708661417322839);
#790=VECTOR('',#2716,18.);
#791=VECTOR('',#2719,36.6456692913386);
#792=VECTOR('',#2720,36.6456692913386);
#793=VECTOR('',#2721,18.);
#794=VECTOR('',#2724,0.708661417322839);
#795=VECTOR('',#2725,0.708661417322839);
#796=VECTOR('',#2734,34.9370078740157);
#797=VECTOR('',#2735,0.708661417322831);
#798=VECTOR('',#2736,34.9370078740157);
#799=VECTOR('',#2737,0.708661417322831);
#800=VECTOR('',#2740,0.708661417322831);
#801=VECTOR('',#2741,34.9370078740157);
#802=VECTOR('',#2742,0.708661417322831);
#803=VECTOR('',#2743,34.9370078740157);
#804=VECTOR('',#2746,21.2913385826772);
#805=VECTOR('',#2747,21.2913385826772);
#806=VECTOR('',#2750,21.2913385826772);
#807=VECTOR('',#2753,21.2913385826772);
#808=VECTOR('',#2760,21.2913385826772);
#809=VECTOR('',#2761,24.6456692913386);
#810=VECTOR('',#2762,21.2913385826772);
#811=VECTOR('',#2763,24.6456692913386);
#812=VECTOR('',#2766,21.2913385826772);
#813=VECTOR('',#2767,0.708661417322836);
#814=VECTOR('',#2768,0.708661417322836);
#815=VECTOR('',#2771,24.6456692913386);
#816=VECTOR('',#2772,24.6456692913386);
#817=VECTOR('',#2773,21.2913385826772);
#818=VECTOR('',#2776,0.708661417322836);
#819=VECTOR('',#2777,0.708661417322836);
#820=VECTOR('',#2788,1.96850393700787);
#821=VECTOR('',#2799,34.9370078740157);
#822=VECTOR('',#2800,0.708661417322833);
#823=VECTOR('',#2801,34.9370078740157);
#824=VECTOR('',#2802,0.708661417322833);
#825=VECTOR('',#2805,0.708661417322833);
#826=VECTOR('',#2806,34.9370078740157);
#827=VECTOR('',#2807,0.708661417322833);
#828=VECTOR('',#2808,34.9370078740157);
#829=VECTOR('',#2811,21.2913385826772);
#830=VECTOR('',#2812,21.2913385826772);
#831=VECTOR('',#2815,21.2913385826772);
#832=VECTOR('',#2818,21.2913385826772);
#833=VECTOR('',#2825,0.708661417322839);
#834=VECTOR('',#2826,18.);
#835=VECTOR('',#2827,0.708661417322839);
#836=VECTOR('',#2828,18.);
#837=VECTOR('',#2831,34.9370078740157);
#838=VECTOR('',#2832,18.);
#839=VECTOR('',#2833,34.9370078740157);
#840=VECTOR('',#2836,0.708661417322839);
#841=VECTOR('',#2837,18.);
#842=VECTOR('',#2838,0.708661417322839);
#843=VECTOR('',#2841,34.9370078740157);
#844=VECTOR('',#2842,34.9370078740157);
#845=VECTOR('',#2851,0.708661417322833);
#846=VECTOR('',#2852,18.);
#847=VECTOR('',#2853,0.708661417322833);
#848=VECTOR('',#2854,18.);
#849=VECTOR('',#2857,11.6456692913386);
#850=VECTOR('',#2858,11.6456692913386);
#851=VECTOR('',#2859,18.);
#852=VECTOR('',#2862,0.708661417322845);
#853=VECTOR('',#2863,0.708661417322845);
#854=VECTOR('',#2864,18.);
#855=VECTOR('',#2867,11.6456692913386);
#856=VECTOR('',#2868,11.6456692913386);
#857=VECTOR('',#2877,41.6456692913386);
#858=VECTOR('',#2878,18.);
#859=VECTOR('',#2879,41.6456692913386);
#860=VECTOR('',#2880,18.);
#861=VECTOR('',#2883,0.708661417322838);
#862=VECTOR('',#2884,0.708661417322838);
#863=VECTOR('',#2885,18.);
#864=VECTOR('',#2888,41.6456692913386);
#865=VECTOR('',#2889,41.6456692913386);
#866=VECTOR('',#2890,18.);
#867=VECTOR('',#2893,0.708661417322836);
#868=VECTOR('',#2894,0.708661417322836);
#869=VECTOR('',#2903,22.);
#870=VECTOR('',#2904,0.708661417322828);
#871=VECTOR('',#2905,22.);
#872=VECTOR('',#2906,0.708661417322828);
#873=VECTOR('',#2909,72.);
#874=VECTOR('',#2910,0.708661417322828);
#875=VECTOR('',#2911,72.);
#876=VECTOR('',#2914,22.);
#877=VECTOR('',#2915,0.708661417322828);
#878=VECTOR('',#2916,22.);
#879=VECTOR('',#2919,72.);
#880=VECTOR('',#2920,72.);
#881=VECTOR('',#2931,1.96850393700787);
#882=VECTOR('',#2944,1.96850393700787);
#883=VECTOR('',#2957,1.96850393700787);
#884=VECTOR('',#2970,1.96850393700787);
#885=VECTOR('',#2981,74.6456692913386);
#886=VECTOR('',#2982,0.708661417322834);
#887=VECTOR('',#2983,74.6456692913386);
#888=VECTOR('',#2984,0.708661417322834);
#889=VECTOR('',#2987,34.9370078740157);
#890=VECTOR('',#2988,0.708661417322834);
#891=VECTOR('',#2989,34.9370078740157);
#892=VECTOR('',#2992,74.6456692913386);
#893=VECTOR('',#2993,0.708661417322834);
#894=VECTOR('',#2994,74.6456692913386);
#895=VECTOR('',#2997,34.9370078740157);
#896=VECTOR('',#2998,34.9370078740157);
#897=VECTOR('',#3007,22.);
#898=VECTOR('',#3008,0.708661417322835);
#899=VECTOR('',#3009,22.);
#900=VECTOR('',#3010,0.708661417322835);
#901=VECTOR('',#3013,72.);
#902=VECTOR('',#3014,0.708661417322835);
#903=VECTOR('',#3015,72.);
#904=VECTOR('',#3018,22.);
#905=VECTOR('',#3019,0.708661417322835);
#906=VECTOR('',#3020,22.);
#907=VECTOR('',#3023,72.);
#908=VECTOR('',#3024,72.);
#909=VECTOR('',#3033,74.6456692913386);
#910=VECTOR('',#3034,0.708661417322834);
#911=VECTOR('',#3035,74.6456692913386);
#912=VECTOR('',#3036,0.708661417322834);
#913=VECTOR('',#3039,34.9370078740157);
#914=VECTOR('',#3040,0.708661417322834);
#915=VECTOR('',#3041,34.9370078740157);
#916=VECTOR('',#3044,74.6456692913386);
#917=VECTOR('',#3045,0.708661417322834);
#918=VECTOR('',#3046,74.6456692913386);
#919=VECTOR('',#3049,34.9370078740157);
#920=VECTOR('',#3050,34.9370078740157);
#921=VERTEX_POINT('',#3107);
#922=VERTEX_POINT('',#3108);
#923=VERTEX_POINT('',#3110);
#924=VERTEX_POINT('',#3112);
#925=VERTEX_POINT('',#3116);
#926=VERTEX_POINT('',#3118);
#927=VERTEX_POINT('',#3122);
#928=VERTEX_POINT('',#3124);
#929=VERTEX_POINT('',#3135);
#930=VERTEX_POINT('',#3136);
#931=VERTEX_POINT('',#3138);
#932=VERTEX_POINT('',#3140);
#933=VERTEX_POINT('',#3144);
#934=VERTEX_POINT('',#3146);
#935=VERTEX_POINT('',#3150);
#936=VERTEX_POINT('',#3152);
#937=VERTEX_POINT('',#3162);
#938=VERTEX_POINT('',#3163);
#939=VERTEX_POINT('',#3165);
#940=VERTEX_POINT('',#3167);
#941=VERTEX_POINT('',#3171);
#942=VERTEX_POINT('',#3173);
#943=VERTEX_POINT('',#3177);
#944=VERTEX_POINT('',#3179);
#945=VERTEX_POINT('',#3189);
#946=VERTEX_POINT('',#3190);
#947=VERTEX_POINT('',#3192);
#948=VERTEX_POINT('',#3194);
#949=VERTEX_POINT('',#3198);
#950=VERTEX_POINT('',#3200);
#951=VERTEX_POINT('',#3204);
#952=VERTEX_POINT('',#3206);
#953=VERTEX_POINT('',#3216);
#954=VERTEX_POINT('',#3218);
#955=VERTEX_POINT('',#3225);
#956=VERTEX_POINT('',#3226);
#957=VERTEX_POINT('',#3228);
#958=VERTEX_POINT('',#3230);
#959=VERTEX_POINT('',#3234);
#960=VERTEX_POINT('',#3236);
#961=VERTEX_POINT('',#3240);
#962=VERTEX_POINT('',#3242);
#963=VERTEX_POINT('',#3252);
#964=VERTEX_POINT('',#3253);
#965=VERTEX_POINT('',#3255);
#966=VERTEX_POINT('',#3257);
#967=VERTEX_POINT('',#3261);
#968=VERTEX_POINT('',#3263);
#969=VERTEX_POINT('',#3267);
#970=VERTEX_POINT('',#3269);
#971=VERTEX_POINT('',#3279);
#972=VERTEX_POINT('',#3280);
#973=VERTEX_POINT('',#3282);
#974=VERTEX_POINT('',#3284);
#975=VERTEX_POINT('',#3288);
#976=VERTEX_POINT('',#3290);
#977=VERTEX_POINT('',#3294);
#978=VERTEX_POINT('',#3296);
#979=VERTEX_POINT('',#3306);
#980=VERTEX_POINT('',#3307);
#981=VERTEX_POINT('',#3309);
#982=VERTEX_POINT('',#3311);
#983=VERTEX_POINT('',#3315);
#984=VERTEX_POINT('',#3317);
#985=VERTEX_POINT('',#3321);
#986=VERTEX_POINT('',#3323);
#987=VERTEX_POINT('',#3333);
#988=VERTEX_POINT('',#3334);
#989=VERTEX_POINT('',#3336);
#990=VERTEX_POINT('',#3338);
#991=VERTEX_POINT('',#3342);
#992=VERTEX_POINT('',#3343);
#993=VERTEX_POINT('',#3345);
#994=VERTEX_POINT('',#3347);
#995=VERTEX_POINT('',#3360);
#996=VERTEX_POINT('',#3361);
#997=VERTEX_POINT('',#3363);
#998=VERTEX_POINT('',#3365);
#999=VERTEX_POINT('',#3369);
#1000=VERTEX_POINT('',#3370);
#1001=VERTEX_POINT('',#3375);
#1002=VERTEX_POINT('',#3377);
#1003=VERTEX_POINT('',#3387);
#1004=VERTEX_POINT('',#3389);
#1005=VERTEX_POINT('',#3396);
#1006=VERTEX_POINT('',#3397);
#1007=VERTEX_POINT('',#3399);
#1008=VERTEX_POINT('',#3401);
#1009=VERTEX_POINT('',#3405);
#1010=VERTEX_POINT('',#3406);
#1011=VERTEX_POINT('',#3408);
#1012=VERTEX_POINT('',#3410);
#1013=VERTEX_POINT('',#3423);
#1014=VERTEX_POINT('',#3424);
#1015=VERTEX_POINT('',#3426);
#1016=VERTEX_POINT('',#3428);
#1017=VERTEX_POINT('',#3432);
#1018=VERTEX_POINT('',#3434);
#1019=VERTEX_POINT('',#3438);
#1020=VERTEX_POINT('',#3440);
#1021=VERTEX_POINT('',#3450);
#1022=VERTEX_POINT('',#3451);
#1023=VERTEX_POINT('',#3453);
#1024=VERTEX_POINT('',#3455);
#1025=VERTEX_POINT('',#3459);
#1026=VERTEX_POINT('',#3461);
#1027=VERTEX_POINT('',#3465);
#1028=VERTEX_POINT('',#3467);
#1029=VERTEX_POINT('',#3477);
#1030=VERTEX_POINT('',#3478);
#1031=VERTEX_POINT('',#3480);
#1032=VERTEX_POINT('',#3482);
#1033=VERTEX_POINT('',#3486);
#1034=VERTEX_POINT('',#3488);
#1035=VERTEX_POINT('',#3492);
#1036=VERTEX_POINT('',#3494);
#1037=VERTEX_POINT('',#3504);
#1038=VERTEX_POINT('',#3505);
#1039=VERTEX_POINT('',#3507);
#1040=VERTEX_POINT('',#3509);
#1041=VERTEX_POINT('',#3513);
#1042=VERTEX_POINT('',#3515);
#1043=VERTEX_POINT('',#3519);
#1044=VERTEX_POINT('',#3521);
#1045=VERTEX_POINT('',#3531);
#1046=VERTEX_POINT('',#3533);
#1047=VERTEX_POINT('',#3540);
#1048=VERTEX_POINT('',#3542);
#1049=VERTEX_POINT('',#3549);
#1050=VERTEX_POINT('',#3551);
#1051=VERTEX_POINT('',#3558);
#1052=VERTEX_POINT('',#3560);
#1053=VERTEX_POINT('',#3567);
#1054=VERTEX_POINT('',#3568);
#1055=VERTEX_POINT('',#3570);
#1056=VERTEX_POINT('',#3572);
#1057=VERTEX_POINT('',#3576);
#1058=VERTEX_POINT('',#3578);
#1059=VERTEX_POINT('',#3582);
#1060=VERTEX_POINT('',#3584);
#1061=VERTEX_POINT('',#3594);
#1062=VERTEX_POINT('',#3595);
#1063=VERTEX_POINT('',#3597);
#1064=VERTEX_POINT('',#3599);
#1065=VERTEX_POINT('',#3603);
#1066=VERTEX_POINT('',#3605);
#1067=VERTEX_POINT('',#3609);
#1068=VERTEX_POINT('',#3611);
#1069=VERTEX_POINT('',#3621);
#1070=VERTEX_POINT('',#3622);
#1071=VERTEX_POINT('',#3624);
#1072=VERTEX_POINT('',#3626);
#1073=VERTEX_POINT('',#3630);
#1074=VERTEX_POINT('',#3632);
#1075=VERTEX_POINT('',#3636);
#1076=VERTEX_POINT('',#3638);
#1077=EDGE_CURVE('',#921,#922,#477,.T.);
#1078=EDGE_CURVE('',#923,#922,#478,.T.);
#1079=EDGE_CURVE('',#924,#923,#479,.T.);
#1080=EDGE_CURVE('',#924,#921,#480,.T.);
#1081=EDGE_CURVE('',#922,#925,#481,.T.);
#1082=EDGE_CURVE('',#926,#925,#482,.T.);
#1083=EDGE_CURVE('',#923,#926,#483,.T.);
#1084=EDGE_CURVE('',#925,#927,#484,.T.);
#1085=EDGE_CURVE('',#928,#927,#485,.T.);
#1086=EDGE_CURVE('',#926,#928,#486,.T.);
#1087=EDGE_CURVE('',#927,#921,#487,.T.);
#1088=EDGE_CURVE('',#928,#924,#488,.T.);
#1089=EDGE_CURVE('',#929,#930,#489,.T.);
#1090=EDGE_CURVE('',#931,#930,#490,.T.);
#1091=EDGE_CURVE('',#932,#931,#491,.T.);
#1092=EDGE_CURVE('',#932,#929,#492,.T.);
#1093=EDGE_CURVE('',#930,#933,#493,.T.);
#1094=EDGE_CURVE('',#934,#933,#494,.T.);
#1095=EDGE_CURVE('',#931,#934,#495,.T.);
#1096=EDGE_CURVE('',#933,#935,#496,.T.);
#1097=EDGE_CURVE('',#936,#935,#497,.T.);
#1098=EDGE_CURVE('',#934,#936,#498,.T.);
#1099=EDGE_CURVE('',#935,#929,#499,.T.);
#1100=EDGE_CURVE('',#936,#932,#500,.T.);
#1101=EDGE_CURVE('',#937,#938,#501,.T.);
#1102=EDGE_CURVE('',#939,#938,#502,.T.);
#1103=EDGE_CURVE('',#940,#939,#503,.T.);
#1104=EDGE_CURVE('',#940,#937,#504,.T.);
#1105=EDGE_CURVE('',#938,#941,#505,.T.);
#1106=EDGE_CURVE('',#942,#941,#506,.T.);
#1107=EDGE_CURVE('',#939,#942,#507,.T.);
#1108=EDGE_CURVE('',#941,#943,#508,.T.);
#1109=EDGE_CURVE('',#944,#943,#509,.T.);
#1110=EDGE_CURVE('',#942,#944,#510,.T.);
#1111=EDGE_CURVE('',#943,#937,#511,.T.);
#1112=EDGE_CURVE('',#944,#940,#512,.T.);
#1113=EDGE_CURVE('',#945,#946,#513,.T.);
#1114=EDGE_CURVE('',#945,#947,#514,.T.);
#1115=EDGE_CURVE('',#947,#948,#515,.T.);
#1116=EDGE_CURVE('',#946,#948,#516,.T.);
#1117=EDGE_CURVE('',#946,#949,#517,.T.);
#1118=EDGE_CURVE('',#948,#950,#518,.T.);
#1119=EDGE_CURVE('',#949,#950,#519,.T.);
#1120=EDGE_CURVE('',#949,#951,#520,.T.);
#1121=EDGE_CURVE('',#950,#952,#521,.T.);
#1122=EDGE_CURVE('',#951,#952,#522,.T.);
#1123=EDGE_CURVE('',#951,#945,#523,.T.);
#1124=EDGE_CURVE('',#952,#947,#524,.T.);
#1125=EDGE_CURVE('',#953,#953,#11,.T.);
#1126=EDGE_CURVE('',#953,#954,#525,.T.);
#1127=EDGE_CURVE('',#954,#954,#12,.T.);
#1128=EDGE_CURVE('',#955,#956,#526,.T.);
#1129=EDGE_CURVE('',#955,#957,#527,.T.);
#1130=EDGE_CURVE('',#957,#958,#528,.T.);
#1131=EDGE_CURVE('',#956,#958,#529,.T.);
#1132=EDGE_CURVE('',#955,#959,#530,.T.);
#1133=EDGE_CURVE('',#956,#960,#531,.T.);
#1134=EDGE_CURVE('',#959,#960,#532,.T.);
#1135=EDGE_CURVE('',#959,#961,#533,.T.);
#1136=EDGE_CURVE('',#960,#962,#534,.T.);
#1137=EDGE_CURVE('',#961,#962,#535,.T.);
#1138=EDGE_CURVE('',#961,#957,#536,.T.);
#1139=EDGE_CURVE('',#962,#958,#537,.T.);
#1140=EDGE_CURVE('',#963,#964,#538,.T.);
#1141=EDGE_CURVE('',#965,#963,#539,.T.);
#1142=EDGE_CURVE('',#965,#966,#540,.T.);
#1143=EDGE_CURVE('',#966,#964,#541,.T.);
#1144=EDGE_CURVE('',#967,#963,#542,.T.);
#1145=EDGE_CURVE('',#968,#967,#543,.T.);
#1146=EDGE_CURVE('',#968,#965,#544,.T.);
#1147=EDGE_CURVE('',#967,#969,#545,.T.);
#1148=EDGE_CURVE('',#970,#969,#546,.T.);
#1149=EDGE_CURVE('',#968,#970,#547,.T.);
#1150=EDGE_CURVE('',#969,#964,#548,.T.);
#1151=EDGE_CURVE('',#970,#966,#549,.T.);
#1152=EDGE_CURVE('',#971,#972,#550,.T.);
#1153=EDGE_CURVE('',#971,#973,#551,.T.);
#1154=EDGE_CURVE('',#973,#974,#552,.T.);
#1155=EDGE_CURVE('',#972,#974,#553,.T.);
#1156=EDGE_CURVE('',#972,#975,#554,.T.);
#1157=EDGE_CURVE('',#974,#976,#555,.T.);
#1158=EDGE_CURVE('',#975,#976,#556,.T.);
#1159=EDGE_CURVE('',#975,#977,#557,.T.);
#1160=EDGE_CURVE('',#976,#978,#558,.T.);
#1161=EDGE_CURVE('',#977,#978,#559,.T.);
#1162=EDGE_CURVE('',#977,#971,#560,.T.);
#1163=EDGE_CURVE('',#978,#973,#561,.T.);
#1164=EDGE_CURVE('',#979,#980,#562,.T.);
#1165=EDGE_CURVE('',#979,#981,#563,.T.);
#1166=EDGE_CURVE('',#981,#982,#564,.T.);
#1167=EDGE_CURVE('',#980,#982,#565,.T.);
#1168=EDGE_CURVE('',#980,#983,#566,.T.);
#1169=EDGE_CURVE('',#982,#984,#567,.T.);
#1170=EDGE_CURVE('',#983,#984,#568,.T.);
#1171=EDGE_CURVE('',#983,#985,#569,.T.);
#1172=EDGE_CURVE('',#984,#986,#570,.T.);
#1173=EDGE_CURVE('',#985,#986,#571,.T.);
#1174=EDGE_CURVE('',#985,#979,#572,.T.);
#1175=EDGE_CURVE('',#986,#981,#573,.T.);
#1176=EDGE_CURVE('',#987,#988,#574,.T.);
#1177=EDGE_CURVE('',#987,#989,#575,.T.);
#1178=EDGE_CURVE('',#989,#990,#576,.T.);
#1179=EDGE_CURVE('',#988,#990,#577,.T.);
#1180=EDGE_CURVE('',#991,#992,#578,.T.);
#1181=EDGE_CURVE('',#991,#993,#579,.T.);
#1182=EDGE_CURVE('',#993,#994,#580,.T.);
#1183=EDGE_CURVE('',#992,#994,#581,.T.);
#1184=EDGE_CURVE('',#987,#991,#582,.T.);
#1185=EDGE_CURVE('',#988,#993,#583,.T.);
#1186=EDGE_CURVE('',#990,#994,#584,.T.);
#1187=EDGE_CURVE('',#989,#992,#585,.T.);
#1188=EDGE_CURVE('',#995,#996,#586,.T.);
#1189=EDGE_CURVE('',#995,#997,#587,.T.);
#1190=EDGE_CURVE('',#997,#998,#588,.T.);
#1191=EDGE_CURVE('',#996,#998,#589,.T.);
#1192=EDGE_CURVE('',#999,#1000,#590,.T.);
#1193=EDGE_CURVE('',#999,#995,#591,.T.);
#1194=EDGE_CURVE('',#1000,#996,#592,.T.);
#1195=EDGE_CURVE('',#999,#1001,#593,.T.);
#1196=EDGE_CURVE('',#1000,#1002,#594,.T.);
#1197=EDGE_CURVE('',#1001,#1002,#595,.T.);
#1198=EDGE_CURVE('',#1001,#997,#596,.T.);
#1199=EDGE_CURVE('',#1002,#998,#597,.T.);
#1200=EDGE_CURVE('',#1003,#1003,#13,.T.);
#1201=EDGE_CURVE('',#1003,#1004,#598,.T.);
#1202=EDGE_CURVE('',#1004,#1004,#14,.T.);
#1203=EDGE_CURVE('',#1005,#1006,#599,.T.);
#1204=EDGE_CURVE('',#1005,#1007,#600,.T.);
#1205=EDGE_CURVE('',#1007,#1008,#601,.T.);
#1206=EDGE_CURVE('',#1006,#1008,#602,.T.);
#1207=EDGE_CURVE('',#1009,#1010,#603,.T.);
#1208=EDGE_CURVE('',#1009,#1011,#604,.T.);
#1209=EDGE_CURVE('',#1011,#1012,#605,.T.);
#1210=EDGE_CURVE('',#1010,#1012,#606,.T.);
#1211=EDGE_CURVE('',#1005,#1009,#607,.T.);
#1212=EDGE_CURVE('',#1006,#1011,#608,.T.);
#1213=EDGE_CURVE('',#1008,#1012,#609,.T.);
#1214=EDGE_CURVE('',#1007,#1010,#610,.T.);
#1215=EDGE_CURVE('',#1013,#1014,#611,.T.);
#1216=EDGE_CURVE('',#1015,#1014,#612,.T.);
#1217=EDGE_CURVE('',#1016,#1015,#613,.T.);
#1218=EDGE_CURVE('',#1016,#1013,#614,.T.);
#1219=EDGE_CURVE('',#1014,#1017,#615,.T.);
#1220=EDGE_CURVE('',#1018,#1017,#616,.T.);
#1221=EDGE_CURVE('',#1015,#1018,#617,.T.);
#1222=EDGE_CURVE('',#1017,#1019,#618,.T.);
#1223=EDGE_CURVE('',#1020,#1019,#619,.T.);
#1224=EDGE_CURVE('',#1018,#1020,#620,.T.);
#1225=EDGE_CURVE('',#1013,#1019,#621,.T.);
#1226=EDGE_CURVE('',#1016,#1020,#622,.T.);
#1227=EDGE_CURVE('',#1021,#1022,#623,.T.);
#1228=EDGE_CURVE('',#1021,#1023,#624,.T.);
#1229=EDGE_CURVE('',#1023,#1024,#625,.T.);
#1230=EDGE_CURVE('',#1022,#1024,#626,.T.);
#1231=EDGE_CURVE('',#1022,#1025,#627,.T.);
#1232=EDGE_CURVE('',#1024,#1026,#628,.T.);
#1233=EDGE_CURVE('',#1025,#1026,#629,.T.);
#1234=EDGE_CURVE('',#1025,#1027,#630,.T.);
#1235=EDGE_CURVE('',#1026,#1028,#631,.T.);
#1236=EDGE_CURVE('',#1027,#1028,#632,.T.);
#1237=EDGE_CURVE('',#1027,#1021,#633,.T.);
#1238=EDGE_CURVE('',#1028,#1023,#634,.T.);
#1239=EDGE_CURVE('',#1029,#1030,#635,.T.);
#1240=EDGE_CURVE('',#1029,#1031,#636,.T.);
#1241=EDGE_CURVE('',#1031,#1032,#637,.T.);
#1242=EDGE_CURVE('',#1030,#1032,#638,.T.);
#1243=EDGE_CURVE('',#1030,#1033,#639,.T.);
#1244=EDGE_CURVE('',#1032,#1034,#640,.T.);
#1245=EDGE_CURVE('',#1033,#1034,#641,.T.);
#1246=EDGE_CURVE('',#1033,#1035,#642,.T.);
#1247=EDGE_CURVE('',#1034,#1036,#643,.T.);
#1248=EDGE_CURVE('',#1035,#1036,#644,.T.);
#1249=EDGE_CURVE('',#1035,#1029,#645,.T.);
#1250=EDGE_CURVE('',#1036,#1031,#646,.T.);
#1251=EDGE_CURVE('',#1037,#1038,#647,.T.);
#1252=EDGE_CURVE('',#1039,#1038,#648,.T.);
#1253=EDGE_CURVE('',#1040,#1039,#649,.T.);
#1254=EDGE_CURVE('',#1040,#1037,#650,.T.);
#1255=EDGE_CURVE('',#1038,#1041,#651,.T.);
#1256=EDGE_CURVE('',#1042,#1041,#652,.T.);
#1257=EDGE_CURVE('',#1039,#1042,#653,.T.);
#1258=EDGE_CURVE('',#1041,#1043,#654,.T.);
#1259=EDGE_CURVE('',#1044,#1043,#655,.T.);
#1260=EDGE_CURVE('',#1042,#1044,#656,.T.);
#1261=EDGE_CURVE('',#1043,#1037,#657,.T.);
#1262=EDGE_CURVE('',#1044,#1040,#658,.T.);
#1263=EDGE_CURVE('',#1045,#1045,#15,.T.);
#1264=EDGE_CURVE('',#1045,#1046,#659,.T.);
#1265=EDGE_CURVE('',#1046,#1046,#16,.T.);
#1266=EDGE_CURVE('',#1047,#1047,#17,.T.);
#1267=EDGE_CURVE('',#1047,#1048,#660,.T.);
#1268=EDGE_CURVE('',#1048,#1048,#18,.T.);
#1269=EDGE_CURVE('',#1049,#1049,#19,.T.);
#1270=EDGE_CURVE('',#1049,#1050,#661,.T.);
#1271=EDGE_CURVE('',#1050,#1050,#20,.T.);
#1272=EDGE_CURVE('',#1051,#1051,#21,.T.);
#1273=EDGE_CURVE('',#1051,#1052,#662,.T.);
#1274=EDGE_CURVE('',#1052,#1052,#22,.T.);
#1275=EDGE_CURVE('',#1053,#1054,#663,.T.);
#1276=EDGE_CURVE('',#1055,#1054,#664,.T.);
#1277=EDGE_CURVE('',#1056,#1055,#665,.T.);
#1278=EDGE_CURVE('',#1056,#1053,#666,.T.);
#1279=EDGE_CURVE('',#1054,#1057,#667,.T.);
#1280=EDGE_CURVE('',#1058,#1057,#668,.T.);
#1281=EDGE_CURVE('',#1055,#1058,#669,.T.);
#1282=EDGE_CURVE('',#1057,#1059,#670,.T.);
#1283=EDGE_CURVE('',#1060,#1059,#671,.T.);
#1284=EDGE_CURVE('',#1058,#1060,#672,.T.);
#1285=EDGE_CURVE('',#1059,#1053,#673,.T.);
#1286=EDGE_CURVE('',#1060,#1056,#674,.T.);
#1287=EDGE_CURVE('',#1061,#1062,#675,.T.);
#1288=EDGE_CURVE('',#1063,#1062,#676,.T.);
#1289=EDGE_CURVE('',#1064,#1063,#677,.T.);
#1290=EDGE_CURVE('',#1064,#1061,#678,.T.);
#1291=EDGE_CURVE('',#1062,#1065,#679,.T.);
#1292=EDGE_CURVE('',#1066,#1065,#680,.T.);
#1293=EDGE_CURVE('',#1063,#1066,#681,.T.);
#1294=EDGE_CURVE('',#1065,#1067,#682,.T.);
#1295=EDGE_CURVE('',#1068,#1067,#683,.T.);
#1296=EDGE_CURVE('',#1066,#1068,#684,.T.);
#1297=EDGE_CURVE('',#1067,#1061,#685,.T.);
#1298=EDGE_CURVE('',#1068,#1064,#686,.T.);
#1299=EDGE_CURVE('',#1069,#1070,#687,.T.);
#1300=EDGE_CURVE('',#1071,#1070,#688,.T.);
#1301=EDGE_CURVE('',#1072,#1071,#689,.T.);
#1302=EDGE_CURVE('',#1072,#1069,#690,.T.);
#1303=EDGE_CURVE('',#1070,#1073,#691,.T.);
#1304=EDGE_CURVE('',#1074,#1073,#692,.T.);
#1305=EDGE_CURVE('',#1071,#1074,#693,.T.);
#1306=EDGE_CURVE('',#1073,#1075,#694,.T.);
#1307=EDGE_CURVE('',#1076,#1075,#695,.T.);
#1308=EDGE_CURVE('',#1074,#1076,#696,.T.);
#1309=EDGE_CURVE('',#1075,#1069,#697,.T.);
#1310=EDGE_CURVE('',#1076,#1072,#698,.T.);
#1311=ORIENTED_EDGE('',*,*,#1077,.T.);
#1312=ORIENTED_EDGE('',*,*,#1078,.F.);
#1313=ORIENTED_EDGE('',*,*,#1079,.F.);
#1314=ORIENTED_EDGE('',*,*,#1080,.T.);
#1315=ORIENTED_EDGE('',*,*,#1081,.T.);
#1316=ORIENTED_EDGE('',*,*,#1082,.F.);
#1317=ORIENTED_EDGE('',*,*,#1083,.F.);
#1318=ORIENTED_EDGE('',*,*,#1078,.T.);
#1319=ORIENTED_EDGE('',*,*,#1084,.T.);
#1320=ORIENTED_EDGE('',*,*,#1085,.F.);
#1321=ORIENTED_EDGE('',*,*,#1086,.F.);
#1322=ORIENTED_EDGE('',*,*,#1082,.T.);
#1323=ORIENTED_EDGE('',*,*,#1087,.T.);
#1324=ORIENTED_EDGE('',*,*,#1080,.F.);
#1325=ORIENTED_EDGE('',*,*,#1088,.F.);
#1326=ORIENTED_EDGE('',*,*,#1085,.T.);
#1327=ORIENTED_EDGE('',*,*,#1079,.T.);
#1328=ORIENTED_EDGE('',*,*,#1083,.T.);
#1329=ORIENTED_EDGE('',*,*,#1086,.T.);
#1330=ORIENTED_EDGE('',*,*,#1088,.T.);
#1331=ORIENTED_EDGE('',*,*,#1077,.F.);
#1332=ORIENTED_EDGE('',*,*,#1087,.F.);
#1333=ORIENTED_EDGE('',*,*,#1084,.F.);
#1334=ORIENTED_EDGE('',*,*,#1081,.F.);
#1335=ORIENTED_EDGE('',*,*,#1089,.T.);
#1336=ORIENTED_EDGE('',*,*,#1090,.F.);
#1337=ORIENTED_EDGE('',*,*,#1091,.F.);
#1338=ORIENTED_EDGE('',*,*,#1092,.T.);
#1339=ORIENTED_EDGE('',*,*,#1093,.T.);
#1340=ORIENTED_EDGE('',*,*,#1094,.F.);
#1341=ORIENTED_EDGE('',*,*,#1095,.F.);
#1342=ORIENTED_EDGE('',*,*,#1090,.T.);
#1343=ORIENTED_EDGE('',*,*,#1096,.T.);
#1344=ORIENTED_EDGE('',*,*,#1097,.F.);
#1345=ORIENTED_EDGE('',*,*,#1098,.F.);
#1346=ORIENTED_EDGE('',*,*,#1094,.T.);
#1347=ORIENTED_EDGE('',*,*,#1099,.T.);
#1348=ORIENTED_EDGE('',*,*,#1092,.F.);
#1349=ORIENTED_EDGE('',*,*,#1100,.F.);
#1350=ORIENTED_EDGE('',*,*,#1097,.T.);
#1351=ORIENTED_EDGE('',*,*,#1091,.T.);
#1352=ORIENTED_EDGE('',*,*,#1095,.T.);
#1353=ORIENTED_EDGE('',*,*,#1098,.T.);
#1354=ORIENTED_EDGE('',*,*,#1100,.T.);
#1355=ORIENTED_EDGE('',*,*,#1089,.F.);
#1356=ORIENTED_EDGE('',*,*,#1099,.F.);
#1357=ORIENTED_EDGE('',*,*,#1096,.F.);
#1358=ORIENTED_EDGE('',*,*,#1093,.F.);
#1359=ORIENTED_EDGE('',*,*,#1101,.T.);
#1360=ORIENTED_EDGE('',*,*,#1102,.F.);
#1361=ORIENTED_EDGE('',*,*,#1103,.F.);
#1362=ORIENTED_EDGE('',*,*,#1104,.T.);
#1363=ORIENTED_EDGE('',*,*,#1105,.T.);
#1364=ORIENTED_EDGE('',*,*,#1106,.F.);
#1365=ORIENTED_EDGE('',*,*,#1107,.F.);
#1366=ORIENTED_EDGE('',*,*,#1102,.T.);
#1367=ORIENTED_EDGE('',*,*,#1108,.T.);
#1368=ORIENTED_EDGE('',*,*,#1109,.F.);
#1369=ORIENTED_EDGE('',*,*,#1110,.F.);
#1370=ORIENTED_EDGE('',*,*,#1106,.T.);
#1371=ORIENTED_EDGE('',*,*,#1111,.T.);
#1372=ORIENTED_EDGE('',*,*,#1104,.F.);
#1373=ORIENTED_EDGE('',*,*,#1112,.F.);
#1374=ORIENTED_EDGE('',*,*,#1109,.T.);
#1375=ORIENTED_EDGE('',*,*,#1103,.T.);
#1376=ORIENTED_EDGE('',*,*,#1107,.T.);
#1377=ORIENTED_EDGE('',*,*,#1110,.T.);
#1378=ORIENTED_EDGE('',*,*,#1112,.T.);
#1379=ORIENTED_EDGE('',*,*,#1101,.F.);
#1380=ORIENTED_EDGE('',*,*,#1111,.F.);
#1381=ORIENTED_EDGE('',*,*,#1108,.F.);
#1382=ORIENTED_EDGE('',*,*,#1105,.F.);
#1383=ORIENTED_EDGE('',*,*,#1113,.F.);
#1384=ORIENTED_EDGE('',*,*,#1114,.T.);
#1385=ORIENTED_EDGE('',*,*,#1115,.T.);
#1386=ORIENTED_EDGE('',*,*,#1116,.F.);
#1387=ORIENTED_EDGE('',*,*,#1117,.F.);
#1388=ORIENTED_EDGE('',*,*,#1116,.T.);
#1389=ORIENTED_EDGE('',*,*,#1118,.T.);
#1390=ORIENTED_EDGE('',*,*,#1119,.F.);
#1391=ORIENTED_EDGE('',*,*,#1120,.F.);
#1392=ORIENTED_EDGE('',*,*,#1119,.T.);
#1393=ORIENTED_EDGE('',*,*,#1121,.T.);
#1394=ORIENTED_EDGE('',*,*,#1122,.F.);
#1395=ORIENTED_EDGE('',*,*,#1123,.F.);
#1396=ORIENTED_EDGE('',*,*,#1122,.T.);
#1397=ORIENTED_EDGE('',*,*,#1124,.T.);
#1398=ORIENTED_EDGE('',*,*,#1114,.F.);
#1399=ORIENTED_EDGE('',*,*,#1115,.F.);
#1400=ORIENTED_EDGE('',*,*,#1124,.F.);
#1401=ORIENTED_EDGE('',*,*,#1121,.F.);
#1402=ORIENTED_EDGE('',*,*,#1118,.F.);
#1403=ORIENTED_EDGE('',*,*,#1123,.T.);
#1404=ORIENTED_EDGE('',*,*,#1113,.T.);
#1405=ORIENTED_EDGE('',*,*,#1117,.T.);
#1406=ORIENTED_EDGE('',*,*,#1120,.T.);
#1407=ORIENTED_EDGE('',*,*,#1125,.T.);
#1408=ORIENTED_EDGE('',*,*,#1126,.T.);
#1409=ORIENTED_EDGE('',*,*,#1127,.F.);
#1410=ORIENTED_EDGE('',*,*,#1126,.F.);
#1411=ORIENTED_EDGE('',*,*,#1127,.T.);
#1412=ORIENTED_EDGE('',*,*,#1125,.F.);
#1413=ORIENTED_EDGE('',*,*,#1128,.F.);
#1414=ORIENTED_EDGE('',*,*,#1129,.T.);
#1415=ORIENTED_EDGE('',*,*,#1130,.T.);
#1416=ORIENTED_EDGE('',*,*,#1131,.F.);
#1417=ORIENTED_EDGE('',*,*,#1132,.F.);
#1418=ORIENTED_EDGE('',*,*,#1128,.T.);
#1419=ORIENTED_EDGE('',*,*,#1133,.T.);
#1420=ORIENTED_EDGE('',*,*,#1134,.F.);
#1421=ORIENTED_EDGE('',*,*,#1135,.F.);
#1422=ORIENTED_EDGE('',*,*,#1134,.T.);
#1423=ORIENTED_EDGE('',*,*,#1136,.T.);
#1424=ORIENTED_EDGE('',*,*,#1137,.F.);
#1425=ORIENTED_EDGE('',*,*,#1138,.F.);
#1426=ORIENTED_EDGE('',*,*,#1137,.T.);
#1427=ORIENTED_EDGE('',*,*,#1139,.T.);
#1428=ORIENTED_EDGE('',*,*,#1130,.F.);
#1429=ORIENTED_EDGE('',*,*,#1131,.T.);
#1430=ORIENTED_EDGE('',*,*,#1139,.F.);
#1431=ORIENTED_EDGE('',*,*,#1136,.F.);
#1432=ORIENTED_EDGE('',*,*,#1133,.F.);
#1433=ORIENTED_EDGE('',*,*,#1129,.F.);
#1434=ORIENTED_EDGE('',*,*,#1132,.T.);
#1435=ORIENTED_EDGE('',*,*,#1135,.T.);
#1436=ORIENTED_EDGE('',*,*,#1138,.T.);
#1437=ORIENTED_EDGE('',*,*,#1140,.F.);
#1438=ORIENTED_EDGE('',*,*,#1141,.F.);
#1439=ORIENTED_EDGE('',*,*,#1142,.T.);
#1440=ORIENTED_EDGE('',*,*,#1143,.T.);
#1441=ORIENTED_EDGE('',*,*,#1144,.F.);
#1442=ORIENTED_EDGE('',*,*,#1145,.F.);
#1443=ORIENTED_EDGE('',*,*,#1146,.T.);
#1444=ORIENTED_EDGE('',*,*,#1141,.T.);
#1445=ORIENTED_EDGE('',*,*,#1147,.T.);
#1446=ORIENTED_EDGE('',*,*,#1148,.F.);
#1447=ORIENTED_EDGE('',*,*,#1149,.F.);
#1448=ORIENTED_EDGE('',*,*,#1145,.T.);
#1449=ORIENTED_EDGE('',*,*,#1150,.T.);
#1450=ORIENTED_EDGE('',*,*,#1143,.F.);
#1451=ORIENTED_EDGE('',*,*,#1151,.F.);
#1452=ORIENTED_EDGE('',*,*,#1148,.T.);
#1453=ORIENTED_EDGE('',*,*,#1142,.F.);
#1454=ORIENTED_EDGE('',*,*,#1146,.F.);
#1455=ORIENTED_EDGE('',*,*,#1149,.T.);
#1456=ORIENTED_EDGE('',*,*,#1151,.T.);
#1457=ORIENTED_EDGE('',*,*,#1140,.T.);
#1458=ORIENTED_EDGE('',*,*,#1150,.F.);
#1459=ORIENTED_EDGE('',*,*,#1147,.F.);
#1460=ORIENTED_EDGE('',*,*,#1144,.T.);
#1461=ORIENTED_EDGE('',*,*,#1152,.F.);
#1462=ORIENTED_EDGE('',*,*,#1153,.T.);
#1463=ORIENTED_EDGE('',*,*,#1154,.T.);
#1464=ORIENTED_EDGE('',*,*,#1155,.F.);
#1465=ORIENTED_EDGE('',*,*,#1156,.F.);
#1466=ORIENTED_EDGE('',*,*,#1155,.T.);
#1467=ORIENTED_EDGE('',*,*,#1157,.T.);
#1468=ORIENTED_EDGE('',*,*,#1158,.F.);
#1469=ORIENTED_EDGE('',*,*,#1159,.F.);
#1470=ORIENTED_EDGE('',*,*,#1158,.T.);
#1471=ORIENTED_EDGE('',*,*,#1160,.T.);
#1472=ORIENTED_EDGE('',*,*,#1161,.F.);
#1473=ORIENTED_EDGE('',*,*,#1162,.F.);
#1474=ORIENTED_EDGE('',*,*,#1161,.T.);
#1475=ORIENTED_EDGE('',*,*,#1163,.T.);
#1476=ORIENTED_EDGE('',*,*,#1153,.F.);
#1477=ORIENTED_EDGE('',*,*,#1154,.F.);
#1478=ORIENTED_EDGE('',*,*,#1163,.F.);
#1479=ORIENTED_EDGE('',*,*,#1160,.F.);
#1480=ORIENTED_EDGE('',*,*,#1157,.F.);
#1481=ORIENTED_EDGE('',*,*,#1162,.T.);
#1482=ORIENTED_EDGE('',*,*,#1152,.T.);
#1483=ORIENTED_EDGE('',*,*,#1156,.T.);
#1484=ORIENTED_EDGE('',*,*,#1159,.T.);
#1485=ORIENTED_EDGE('',*,*,#1164,.F.);
#1486=ORIENTED_EDGE('',*,*,#1165,.T.);
#1487=ORIENTED_EDGE('',*,*,#1166,.T.);
#1488=ORIENTED_EDGE('',*,*,#1167,.F.);
#1489=ORIENTED_EDGE('',*,*,#1168,.F.);
#1490=ORIENTED_EDGE('',*,*,#1167,.T.);
#1491=ORIENTED_EDGE('',*,*,#1169,.T.);
#1492=ORIENTED_EDGE('',*,*,#1170,.F.);
#1493=ORIENTED_EDGE('',*,*,#1171,.F.);
#1494=ORIENTED_EDGE('',*,*,#1170,.T.);
#1495=ORIENTED_EDGE('',*,*,#1172,.T.);
#1496=ORIENTED_EDGE('',*,*,#1173,.F.);
#1497=ORIENTED_EDGE('',*,*,#1174,.F.);
#1498=ORIENTED_EDGE('',*,*,#1173,.T.);
#1499=ORIENTED_EDGE('',*,*,#1175,.T.);
#1500=ORIENTED_EDGE('',*,*,#1165,.F.);
#1501=ORIENTED_EDGE('',*,*,#1166,.F.);
#1502=ORIENTED_EDGE('',*,*,#1175,.F.);
#1503=ORIENTED_EDGE('',*,*,#1172,.F.);
#1504=ORIENTED_EDGE('',*,*,#1169,.F.);
#1505=ORIENTED_EDGE('',*,*,#1174,.T.);
#1506=ORIENTED_EDGE('',*,*,#1164,.T.);
#1507=ORIENTED_EDGE('',*,*,#1168,.T.);
#1508=ORIENTED_EDGE('',*,*,#1171,.T.);
#1509=ORIENTED_EDGE('',*,*,#1176,.F.);
#1510=ORIENTED_EDGE('',*,*,#1177,.T.);
#1511=ORIENTED_EDGE('',*,*,#1178,.T.);
#1512=ORIENTED_EDGE('',*,*,#1179,.F.);
#1513=ORIENTED_EDGE('',*,*,#1180,.F.);
#1514=ORIENTED_EDGE('',*,*,#1181,.T.);
#1515=ORIENTED_EDGE('',*,*,#1182,.T.);
#1516=ORIENTED_EDGE('',*,*,#1183,.F.);
#1517=ORIENTED_EDGE('',*,*,#1184,.F.);
#1518=ORIENTED_EDGE('',*,*,#1176,.T.);
#1519=ORIENTED_EDGE('',*,*,#1185,.T.);
#1520=ORIENTED_EDGE('',*,*,#1181,.F.);
#1521=ORIENTED_EDGE('',*,*,#1185,.F.);
#1522=ORIENTED_EDGE('',*,*,#1179,.T.);
#1523=ORIENTED_EDGE('',*,*,#1186,.T.);
#1524=ORIENTED_EDGE('',*,*,#1182,.F.);
#1525=ORIENTED_EDGE('',*,*,#1178,.F.);
#1526=ORIENTED_EDGE('',*,*,#1187,.T.);
#1527=ORIENTED_EDGE('',*,*,#1183,.T.);
#1528=ORIENTED_EDGE('',*,*,#1186,.F.);
#1529=ORIENTED_EDGE('',*,*,#1177,.F.);
#1530=ORIENTED_EDGE('',*,*,#1184,.T.);
#1531=ORIENTED_EDGE('',*,*,#1180,.T.);
#1532=ORIENTED_EDGE('',*,*,#1187,.F.);
#1533=ORIENTED_EDGE('',*,*,#1188,.F.);
#1534=ORIENTED_EDGE('',*,*,#1189,.T.);
#1535=ORIENTED_EDGE('',*,*,#1190,.T.);
#1536=ORIENTED_EDGE('',*,*,#1191,.F.);
#1537=ORIENTED_EDGE('',*,*,#1192,.F.);
#1538=ORIENTED_EDGE('',*,*,#1193,.T.);
#1539=ORIENTED_EDGE('',*,*,#1188,.T.);
#1540=ORIENTED_EDGE('',*,*,#1194,.F.);
#1541=ORIENTED_EDGE('',*,*,#1195,.F.);
#1542=ORIENTED_EDGE('',*,*,#1192,.T.);
#1543=ORIENTED_EDGE('',*,*,#1196,.T.);
#1544=ORIENTED_EDGE('',*,*,#1197,.F.);
#1545=ORIENTED_EDGE('',*,*,#1198,.F.);
#1546=ORIENTED_EDGE('',*,*,#1197,.T.);
#1547=ORIENTED_EDGE('',*,*,#1199,.T.);
#1548=ORIENTED_EDGE('',*,*,#1190,.F.);
#1549=ORIENTED_EDGE('',*,*,#1191,.T.);
#1550=ORIENTED_EDGE('',*,*,#1199,.F.);
#1551=ORIENTED_EDGE('',*,*,#1196,.F.);
#1552=ORIENTED_EDGE('',*,*,#1194,.T.);
#1553=ORIENTED_EDGE('',*,*,#1189,.F.);
#1554=ORIENTED_EDGE('',*,*,#1193,.F.);
#1555=ORIENTED_EDGE('',*,*,#1195,.T.);
#1556=ORIENTED_EDGE('',*,*,#1198,.T.);
#1557=ORIENTED_EDGE('',*,*,#1200,.T.);
#1558=ORIENTED_EDGE('',*,*,#1201,.T.);
#1559=ORIENTED_EDGE('',*,*,#1202,.F.);
#1560=ORIENTED_EDGE('',*,*,#1201,.F.);
#1561=ORIENTED_EDGE('',*,*,#1202,.T.);
#1562=ORIENTED_EDGE('',*,*,#1200,.F.);
#1563=ORIENTED_EDGE('',*,*,#1203,.F.);
#1564=ORIENTED_EDGE('',*,*,#1204,.T.);
#1565=ORIENTED_EDGE('',*,*,#1205,.T.);
#1566=ORIENTED_EDGE('',*,*,#1206,.F.);
#1567=ORIENTED_EDGE('',*,*,#1207,.F.);
#1568=ORIENTED_EDGE('',*,*,#1208,.T.);
#1569=ORIENTED_EDGE('',*,*,#1209,.T.);
#1570=ORIENTED_EDGE('',*,*,#1210,.F.);
#1571=ORIENTED_EDGE('',*,*,#1211,.F.);
#1572=ORIENTED_EDGE('',*,*,#1203,.T.);
#1573=ORIENTED_EDGE('',*,*,#1212,.T.);
#1574=ORIENTED_EDGE('',*,*,#1208,.F.);
#1575=ORIENTED_EDGE('',*,*,#1212,.F.);
#1576=ORIENTED_EDGE('',*,*,#1206,.T.);
#1577=ORIENTED_EDGE('',*,*,#1213,.T.);
#1578=ORIENTED_EDGE('',*,*,#1209,.F.);
#1579=ORIENTED_EDGE('',*,*,#1205,.F.);
#1580=ORIENTED_EDGE('',*,*,#1214,.T.);
#1581=ORIENTED_EDGE('',*,*,#1210,.T.);
#1582=ORIENTED_EDGE('',*,*,#1213,.F.);
#1583=ORIENTED_EDGE('',*,*,#1204,.F.);
#1584=ORIENTED_EDGE('',*,*,#1211,.T.);
#1585=ORIENTED_EDGE('',*,*,#1207,.T.);
#1586=ORIENTED_EDGE('',*,*,#1214,.F.);
#1587=ORIENTED_EDGE('',*,*,#1215,.T.);
#1588=ORIENTED_EDGE('',*,*,#1216,.F.);
#1589=ORIENTED_EDGE('',*,*,#1217,.F.);
#1590=ORIENTED_EDGE('',*,*,#1218,.T.);
#1591=ORIENTED_EDGE('',*,*,#1219,.T.);
#1592=ORIENTED_EDGE('',*,*,#1220,.F.);
#1593=ORIENTED_EDGE('',*,*,#1221,.F.);
#1594=ORIENTED_EDGE('',*,*,#1216,.T.);
#1595=ORIENTED_EDGE('',*,*,#1222,.T.);
#1596=ORIENTED_EDGE('',*,*,#1223,.F.);
#1597=ORIENTED_EDGE('',*,*,#1224,.F.);
#1598=ORIENTED_EDGE('',*,*,#1220,.T.);
#1599=ORIENTED_EDGE('',*,*,#1225,.F.);
#1600=ORIENTED_EDGE('',*,*,#1218,.F.);
#1601=ORIENTED_EDGE('',*,*,#1226,.T.);
#1602=ORIENTED_EDGE('',*,*,#1223,.T.);
#1603=ORIENTED_EDGE('',*,*,#1217,.T.);
#1604=ORIENTED_EDGE('',*,*,#1221,.T.);
#1605=ORIENTED_EDGE('',*,*,#1224,.T.);
#1606=ORIENTED_EDGE('',*,*,#1226,.F.);
#1607=ORIENTED_EDGE('',*,*,#1215,.F.);
#1608=ORIENTED_EDGE('',*,*,#1225,.T.);
#1609=ORIENTED_EDGE('',*,*,#1222,.F.);
#1610=ORIENTED_EDGE('',*,*,#1219,.F.);
#1611=ORIENTED_EDGE('',*,*,#1227,.F.);
#1612=ORIENTED_EDGE('',*,*,#1228,.T.);
#1613=ORIENTED_EDGE('',*,*,#1229,.T.);
#1614=ORIENTED_EDGE('',*,*,#1230,.F.);
#1615=ORIENTED_EDGE('',*,*,#1231,.F.);
#1616=ORIENTED_EDGE('',*,*,#1230,.T.);
#1617=ORIENTED_EDGE('',*,*,#1232,.T.);
#1618=ORIENTED_EDGE('',*,*,#1233,.F.);
#1619=ORIENTED_EDGE('',*,*,#1234,.F.);
#1620=ORIENTED_EDGE('',*,*,#1233,.T.);
#1621=ORIENTED_EDGE('',*,*,#1235,.T.);
#1622=ORIENTED_EDGE('',*,*,#1236,.F.);
#1623=ORIENTED_EDGE('',*,*,#1237,.F.);
#1624=ORIENTED_EDGE('',*,*,#1236,.T.);
#1625=ORIENTED_EDGE('',*,*,#1238,.T.);
#1626=ORIENTED_EDGE('',*,*,#1228,.F.);
#1627=ORIENTED_EDGE('',*,*,#1229,.F.);
#1628=ORIENTED_EDGE('',*,*,#1238,.F.);
#1629=ORIENTED_EDGE('',*,*,#1235,.F.);
#1630=ORIENTED_EDGE('',*,*,#1232,.F.);
#1631=ORIENTED_EDGE('',*,*,#1237,.T.);
#1632=ORIENTED_EDGE('',*,*,#1227,.T.);
#1633=ORIENTED_EDGE('',*,*,#1231,.T.);
#1634=ORIENTED_EDGE('',*,*,#1234,.T.);
#1635=ORIENTED_EDGE('',*,*,#1239,.F.);
#1636=ORIENTED_EDGE('',*,*,#1240,.T.);
#1637=ORIENTED_EDGE('',*,*,#1241,.T.);
#1638=ORIENTED_EDGE('',*,*,#1242,.F.);
#1639=ORIENTED_EDGE('',*,*,#1243,.F.);
#1640=ORIENTED_EDGE('',*,*,#1242,.T.);
#1641=ORIENTED_EDGE('',*,*,#1244,.T.);
#1642=ORIENTED_EDGE('',*,*,#1245,.F.);
#1643=ORIENTED_EDGE('',*,*,#1246,.F.);
#1644=ORIENTED_EDGE('',*,*,#1245,.T.);
#1645=ORIENTED_EDGE('',*,*,#1247,.T.);
#1646=ORIENTED_EDGE('',*,*,#1248,.F.);
#1647=ORIENTED_EDGE('',*,*,#1249,.F.);
#1648=ORIENTED_EDGE('',*,*,#1248,.T.);
#1649=ORIENTED_EDGE('',*,*,#1250,.T.);
#1650=ORIENTED_EDGE('',*,*,#1240,.F.);
#1651=ORIENTED_EDGE('',*,*,#1241,.F.);
#1652=ORIENTED_EDGE('',*,*,#1250,.F.);
#1653=ORIENTED_EDGE('',*,*,#1247,.F.);
#1654=ORIENTED_EDGE('',*,*,#1244,.F.);
#1655=ORIENTED_EDGE('',*,*,#1249,.T.);
#1656=ORIENTED_EDGE('',*,*,#1239,.T.);
#1657=ORIENTED_EDGE('',*,*,#1243,.T.);
#1658=ORIENTED_EDGE('',*,*,#1246,.T.);
#1659=ORIENTED_EDGE('',*,*,#1251,.T.);
#1660=ORIENTED_EDGE('',*,*,#1252,.F.);
#1661=ORIENTED_EDGE('',*,*,#1253,.F.);
#1662=ORIENTED_EDGE('',*,*,#1254,.T.);
#1663=ORIENTED_EDGE('',*,*,#1255,.T.);
#1664=ORIENTED_EDGE('',*,*,#1256,.F.);
#1665=ORIENTED_EDGE('',*,*,#1257,.F.);
#1666=ORIENTED_EDGE('',*,*,#1252,.T.);
#1667=ORIENTED_EDGE('',*,*,#1258,.T.);
#1668=ORIENTED_EDGE('',*,*,#1259,.F.);
#1669=ORIENTED_EDGE('',*,*,#1260,.F.);
#1670=ORIENTED_EDGE('',*,*,#1256,.T.);
#1671=ORIENTED_EDGE('',*,*,#1261,.T.);
#1672=ORIENTED_EDGE('',*,*,#1254,.F.);
#1673=ORIENTED_EDGE('',*,*,#1262,.F.);
#1674=ORIENTED_EDGE('',*,*,#1259,.T.);
#1675=ORIENTED_EDGE('',*,*,#1253,.T.);
#1676=ORIENTED_EDGE('',*,*,#1257,.T.);
#1677=ORIENTED_EDGE('',*,*,#1260,.T.);
#1678=ORIENTED_EDGE('',*,*,#1262,.T.);
#1679=ORIENTED_EDGE('',*,*,#1251,.F.);
#1680=ORIENTED_EDGE('',*,*,#1261,.F.);
#1681=ORIENTED_EDGE('',*,*,#1258,.F.);
#1682=ORIENTED_EDGE('',*,*,#1255,.F.);
#1683=ORIENTED_EDGE('',*,*,#1263,.T.);
#1684=ORIENTED_EDGE('',*,*,#1264,.T.);
#1685=ORIENTED_EDGE('',*,*,#1265,.F.);
#1686=ORIENTED_EDGE('',*,*,#1264,.F.);
#1687=ORIENTED_EDGE('',*,*,#1265,.T.);
#1688=ORIENTED_EDGE('',*,*,#1263,.F.);
#1689=ORIENTED_EDGE('',*,*,#1266,.T.);
#1690=ORIENTED_EDGE('',*,*,#1267,.T.);
#1691=ORIENTED_EDGE('',*,*,#1268,.F.);
#1692=ORIENTED_EDGE('',*,*,#1267,.F.);
#1693=ORIENTED_EDGE('',*,*,#1268,.T.);
#1694=ORIENTED_EDGE('',*,*,#1266,.F.);
#1695=ORIENTED_EDGE('',*,*,#1269,.T.);
#1696=ORIENTED_EDGE('',*,*,#1270,.T.);
#1697=ORIENTED_EDGE('',*,*,#1271,.F.);
#1698=ORIENTED_EDGE('',*,*,#1270,.F.);
#1699=ORIENTED_EDGE('',*,*,#1271,.T.);
#1700=ORIENTED_EDGE('',*,*,#1269,.F.);
#1701=ORIENTED_EDGE('',*,*,#1272,.T.);
#1702=ORIENTED_EDGE('',*,*,#1273,.T.);
#1703=ORIENTED_EDGE('',*,*,#1274,.F.);
#1704=ORIENTED_EDGE('',*,*,#1273,.F.);
#1705=ORIENTED_EDGE('',*,*,#1274,.T.);
#1706=ORIENTED_EDGE('',*,*,#1272,.F.);
#1707=ORIENTED_EDGE('',*,*,#1275,.T.);
#1708=ORIENTED_EDGE('',*,*,#1276,.F.);
#1709=ORIENTED_EDGE('',*,*,#1277,.F.);
#1710=ORIENTED_EDGE('',*,*,#1278,.T.);
#1711=ORIENTED_EDGE('',*,*,#1279,.T.);
#1712=ORIENTED_EDGE('',*,*,#1280,.F.);
#1713=ORIENTED_EDGE('',*,*,#1281,.F.);
#1714=ORIENTED_EDGE('',*,*,#1276,.T.);
#1715=ORIENTED_EDGE('',*,*,#1282,.T.);
#1716=ORIENTED_EDGE('',*,*,#1283,.F.);
#1717=ORIENTED_EDGE('',*,*,#1284,.F.);
#1718=ORIENTED_EDGE('',*,*,#1280,.T.);
#1719=ORIENTED_EDGE('',*,*,#1285,.T.);
#1720=ORIENTED_EDGE('',*,*,#1278,.F.);
#1721=ORIENTED_EDGE('',*,*,#1286,.F.);
#1722=ORIENTED_EDGE('',*,*,#1283,.T.);
#1723=ORIENTED_EDGE('',*,*,#1277,.T.);
#1724=ORIENTED_EDGE('',*,*,#1281,.T.);
#1725=ORIENTED_EDGE('',*,*,#1284,.T.);
#1726=ORIENTED_EDGE('',*,*,#1286,.T.);
#1727=ORIENTED_EDGE('',*,*,#1275,.F.);
#1728=ORIENTED_EDGE('',*,*,#1285,.F.);
#1729=ORIENTED_EDGE('',*,*,#1282,.F.);
#1730=ORIENTED_EDGE('',*,*,#1279,.F.);
#1731=ORIENTED_EDGE('',*,*,#1287,.T.);
#1732=ORIENTED_EDGE('',*,*,#1288,.F.);
#1733=ORIENTED_EDGE('',*,*,#1289,.F.);
#1734=ORIENTED_EDGE('',*,*,#1290,.T.);
#1735=ORIENTED_EDGE('',*,*,#1291,.T.);
#1736=ORIENTED_EDGE('',*,*,#1292,.F.);
#1737=ORIENTED_EDGE('',*,*,#1293,.F.);
#1738=ORIENTED_EDGE('',*,*,#1288,.T.);
#1739=ORIENTED_EDGE('',*,*,#1294,.T.);
#1740=ORIENTED_EDGE('',*,*,#1295,.F.);
#1741=ORIENTED_EDGE('',*,*,#1296,.F.);
#1742=ORIENTED_EDGE('',*,*,#1292,.T.);
#1743=ORIENTED_EDGE('',*,*,#1297,.T.);
#1744=ORIENTED_EDGE('',*,*,#1290,.F.);
#1745=ORIENTED_EDGE('',*,*,#1298,.F.);
#1746=ORIENTED_EDGE('',*,*,#1295,.T.);
#1747=ORIENTED_EDGE('',*,*,#1289,.T.);
#1748=ORIENTED_EDGE('',*,*,#1293,.T.);
#1749=ORIENTED_EDGE('',*,*,#1296,.T.);
#1750=ORIENTED_EDGE('',*,*,#1298,.T.);
#1751=ORIENTED_EDGE('',*,*,#1287,.F.);
#1752=ORIENTED_EDGE('',*,*,#1297,.F.);
#1753=ORIENTED_EDGE('',*,*,#1294,.F.);
#1754=ORIENTED_EDGE('',*,*,#1291,.F.);
#1755=ORIENTED_EDGE('',*,*,#1299,.T.);
#1756=ORIENTED_EDGE('',*,*,#1300,.F.);
#1757=ORIENTED_EDGE('',*,*,#1301,.F.);
#1758=ORIENTED_EDGE('',*,*,#1302,.T.);
#1759=ORIENTED_EDGE('',*,*,#1303,.T.);
#1760=ORIENTED_EDGE('',*,*,#1304,.F.);
#1761=ORIENTED_EDGE('',*,*,#1305,.F.);
#1762=ORIENTED_EDGE('',*,*,#1300,.T.);
#1763=ORIENTED_EDGE('',*,*,#1306,.T.);
#1764=ORIENTED_EDGE('',*,*,#1307,.F.);
#1765=ORIENTED_EDGE('',*,*,#1308,.F.);
#1766=ORIENTED_EDGE('',*,*,#1304,.T.);
#1767=ORIENTED_EDGE('',*,*,#1309,.T.);
#1768=ORIENTED_EDGE('',*,*,#1302,.F.);
#1769=ORIENTED_EDGE('',*,*,#1310,.F.);
#1770=ORIENTED_EDGE('',*,*,#1307,.T.);
#1771=ORIENTED_EDGE('',*,*,#1301,.T.);
#1772=ORIENTED_EDGE('',*,*,#1305,.T.);
#1773=ORIENTED_EDGE('',*,*,#1308,.T.);
#1774=ORIENTED_EDGE('',*,*,#1310,.T.);
#1775=ORIENTED_EDGE('',*,*,#1299,.F.);
#1776=ORIENTED_EDGE('',*,*,#1309,.F.);
#1777=ORIENTED_EDGE('',*,*,#1306,.F.);
#1778=ORIENTED_EDGE('',*,*,#1303,.F.);
#1779=PLANE('',#2317);
#1780=PLANE('',#2318);
#1781=PLANE('',#2319);
#1782=PLANE('',#2320);
#1783=PLANE('',#2321);
#1784=PLANE('',#2322);
#1785=PLANE('',#2325);
#1786=PLANE('',#2326);
#1787=PLANE('',#2327);
#1788=PLANE('',#2328);
#1789=PLANE('',#2329);
#1790=PLANE('',#2330);
#1791=PLANE('',#2332);
#1792=PLANE('',#2333);
#1793=PLANE('',#2334);
#1794=PLANE('',#2335);
#1795=PLANE('',#2336);
#1796=PLANE('',#2337);
#1797=PLANE('',#2339);
#1798=PLANE('',#2340);
#1799=PLANE('',#2341);
#1800=PLANE('',#2342);
#1801=PLANE('',#2343);
#1802=PLANE('',#2344);
#1803=PLANE('',#2349);
#1804=PLANE('',#2350);
#1805=PLANE('',#2352);
#1806=PLANE('',#2353);
#1807=PLANE('',#2354);
#1808=PLANE('',#2355);
#1809=PLANE('',#2356);
#1810=PLANE('',#2357);
#1811=PLANE('',#2359);
#1812=PLANE('',#2360);
#1813=PLANE('',#2361);
#1814=PLANE('',#2362);
#1815=PLANE('',#2363);
#1816=PLANE('',#2364);
#1817=PLANE('',#2366);
#1818=PLANE('',#2367);
#1819=PLANE('',#2368);
#1820=PLANE('',#2369);
#1821=PLANE('',#2370);
#1822=PLANE('',#2371);
#1823=PLANE('',#2373);
#1824=PLANE('',#2374);
#1825=PLANE('',#2375);
#1826=PLANE('',#2376);
#1827=PLANE('',#2377);
#1828=PLANE('',#2378);
#1829=PLANE('',#2380);
#1830=PLANE('',#2381);
#1831=PLANE('',#2382);
#1832=PLANE('',#2383);
#1833=PLANE('',#2384);
#1834=PLANE('',#2385);
#1835=PLANE('',#2387);
#1836=PLANE('',#2388);
#1837=PLANE('',#2389);
#1838=PLANE('',#2390);
#1839=PLANE('',#2391);
#1840=PLANE('',#2392);
#1841=PLANE('',#2397);
#1842=PLANE('',#2398);
#1843=PLANE('',#2400);
#1844=PLANE('',#2401);
#1845=PLANE('',#2402);
#1846=PLANE('',#2403);
#1847=PLANE('',#2404);
#1848=PLANE('',#2405);
#1849=PLANE('',#2407);
#1850=PLANE('',#2408);
#1851=PLANE('',#2409);
#1852=PLANE('',#2410);
#1853=PLANE('',#2411);
#1854=PLANE('',#2412);
#1855=PLANE('',#2414);
#1856=PLANE('',#2415);
#1857=PLANE('',#2416);
#1858=PLANE('',#2417);
#1859=PLANE('',#2418);
#1860=PLANE('',#2419);
#1861=PLANE('',#2421);
#1862=PLANE('',#2422);
#1863=PLANE('',#2423);
#1864=PLANE('',#2424);
#1865=PLANE('',#2425);
#1866=PLANE('',#2426);
#1867=PLANE('',#2428);
#1868=PLANE('',#2429);
#1869=PLANE('',#2430);
#1870=PLANE('',#2431);
#1871=PLANE('',#2432);
#1872=PLANE('',#2433);
#1873=PLANE('',#2438);
#1874=PLANE('',#2439);
#1875=PLANE('',#2444);
#1876=PLANE('',#2445);
#1877=PLANE('',#2450);
#1878=PLANE('',#2451);
#1879=PLANE('',#2456);
#1880=PLANE('',#2457);
#1881=PLANE('',#2459);
#1882=PLANE('',#2460);
#1883=PLANE('',#2461);
#1884=PLANE('',#2462);
#1885=PLANE('',#2463);
#1886=PLANE('',#2464);
#1887=PLANE('',#2466);
#1888=PLANE('',#2467);
#1889=PLANE('',#2468);
#1890=PLANE('',#2469);
#1891=PLANE('',#2470);
#1892=PLANE('',#2471);
#1893=PLANE('',#2473);
#1894=PLANE('',#2474);
#1895=PLANE('',#2475);
#1896=PLANE('',#2476);
#1897=PLANE('',#2477);
#1898=PLANE('',#2478);
#1899=ADVANCED_FACE('',(#225),#1779,.F.);
#1900=ADVANCED_FACE('',(#226),#1780,.F.);
#1901=ADVANCED_FACE('',(#227),#1781,.F.);
#1902=ADVANCED_FACE('',(#228),#1782,.F.);
#1903=ADVANCED_FACE('',(#229),#1783,.F.);
#1904=ADVANCED_FACE('',(#230),#1784,.T.);
#1905=ADVANCED_FACE('',(#231),#1785,.F.);
#1906=ADVANCED_FACE('',(#232),#1786,.F.);
#1907=ADVANCED_FACE('',(#233),#1787,.F.);
#1908=ADVANCED_FACE('',(#234),#1788,.F.);
#1909=ADVANCED_FACE('',(#235),#1789,.T.);
#1910=ADVANCED_FACE('',(#236),#1790,.F.);
#1911=ADVANCED_FACE('',(#237),#1791,.F.);
#1912=ADVANCED_FACE('',(#238),#1792,.F.);
#1913=ADVANCED_FACE('',(#239),#1793,.F.);
#1914=ADVANCED_FACE('',(#240),#1794,.F.);
#1915=ADVANCED_FACE('',(#241),#1795,.T.);
#1916=ADVANCED_FACE('',(#242),#1796,.F.);
#1917=ADVANCED_FACE('',(#243),#1797,.F.);
#1918=ADVANCED_FACE('',(#244),#1798,.F.);
#1919=ADVANCED_FACE('',(#245),#1799,.F.);
#1920=ADVANCED_FACE('',(#246),#1800,.F.);
#1921=ADVANCED_FACE('',(#247),#1801,.F.);
#1922=ADVANCED_FACE('',(#248),#1802,.T.);
#1923=ADVANCED_FACE('',(#249),#23,.T.);
#1924=ADVANCED_FACE('',(#250),#1803,.T.);
#1925=ADVANCED_FACE('',(#251),#1804,.F.);
#1926=ADVANCED_FACE('',(#252),#1805,.T.);
#1927=ADVANCED_FACE('',(#253),#1806,.F.);
#1928=ADVANCED_FACE('',(#254),#1807,.F.);
#1929=ADVANCED_FACE('',(#255),#1808,.F.);
#1930=ADVANCED_FACE('',(#256),#1809,.F.);
#1931=ADVANCED_FACE('',(#257),#1810,.T.);
#1932=ADVANCED_FACE('',(#258),#1811,.T.);
#1933=ADVANCED_FACE('',(#259),#1812,.T.);
#1934=ADVANCED_FACE('',(#260),#1813,.F.);
#1935=ADVANCED_FACE('',(#261),#1814,.F.);
#1936=ADVANCED_FACE('',(#262),#1815,.T.);
#1937=ADVANCED_FACE('',(#263),#1816,.F.);
#1938=ADVANCED_FACE('',(#264),#1817,.F.);
#1939=ADVANCED_FACE('',(#265),#1818,.F.);
#1940=ADVANCED_FACE('',(#266),#1819,.F.);
#1941=ADVANCED_FACE('',(#267),#1820,.F.);
#1942=ADVANCED_FACE('',(#268),#1821,.F.);
#1943=ADVANCED_FACE('',(#269),#1822,.T.);
#1944=ADVANCED_FACE('',(#270),#1823,.F.);
#1945=ADVANCED_FACE('',(#271),#1824,.F.);
#1946=ADVANCED_FACE('',(#272),#1825,.F.);
#1947=ADVANCED_FACE('',(#273),#1826,.F.);
#1948=ADVANCED_FACE('',(#274),#1827,.F.);
#1949=ADVANCED_FACE('',(#275),#1828,.T.);
#1950=ADVANCED_FACE('',(#276),#1829,.T.);
#1951=ADVANCED_FACE('',(#277),#1830,.F.);
#1952=ADVANCED_FACE('',(#278),#1831,.T.);
#1953=ADVANCED_FACE('',(#279),#1832,.T.);
#1954=ADVANCED_FACE('',(#280),#1833,.F.);
#1955=ADVANCED_FACE('',(#281),#1834,.F.);
#1956=ADVANCED_FACE('',(#282),#1835,.T.);
#1957=ADVANCED_FACE('',(#283),#1836,.T.);
#1958=ADVANCED_FACE('',(#284),#1837,.F.);
#1959=ADVANCED_FACE('',(#285),#1838,.F.);
#1960=ADVANCED_FACE('',(#286),#1839,.F.);
#1961=ADVANCED_FACE('',(#287),#1840,.T.);
#1962=ADVANCED_FACE('',(#288),#24,.T.);
#1963=ADVANCED_FACE('',(#289),#1841,.T.);
#1964=ADVANCED_FACE('',(#290),#1842,.F.);
#1965=ADVANCED_FACE('',(#291),#1843,.T.);
#1966=ADVANCED_FACE('',(#292),#1844,.F.);
#1967=ADVANCED_FACE('',(#293),#1845,.T.);
#1968=ADVANCED_FACE('',(#294),#1846,.T.);
#1969=ADVANCED_FACE('',(#295),#1847,.F.);
#1970=ADVANCED_FACE('',(#296),#1848,.F.);
#1971=ADVANCED_FACE('',(#297),#1849,.F.);
#1972=ADVANCED_FACE('',(#298),#1850,.F.);
#1973=ADVANCED_FACE('',(#299),#1851,.F.);
#1974=ADVANCED_FACE('',(#300),#1852,.T.);
#1975=ADVANCED_FACE('',(#301),#1853,.T.);
#1976=ADVANCED_FACE('',(#302),#1854,.F.);
#1977=ADVANCED_FACE('',(#303),#1855,.F.);
#1978=ADVANCED_FACE('',(#304),#1856,.F.);
#1979=ADVANCED_FACE('',(#305),#1857,.F.);
#1980=ADVANCED_FACE('',(#306),#1858,.F.);
#1981=ADVANCED_FACE('',(#307),#1859,.F.);
#1982=ADVANCED_FACE('',(#308),#1860,.T.);
#1983=ADVANCED_FACE('',(#309),#1861,.F.);
#1984=ADVANCED_FACE('',(#310),#1862,.F.);
#1985=ADVANCED_FACE('',(#311),#1863,.F.);
#1986=ADVANCED_FACE('',(#312),#1864,.F.);
#1987=ADVANCED_FACE('',(#313),#1865,.F.);
#1988=ADVANCED_FACE('',(#314),#1866,.T.);
#1989=ADVANCED_FACE('',(#315),#1867,.F.);
#1990=ADVANCED_FACE('',(#316),#1868,.F.);
#1991=ADVANCED_FACE('',(#317),#1869,.F.);
#1992=ADVANCED_FACE('',(#318),#1870,.F.);
#1993=ADVANCED_FACE('',(#319),#1871,.T.);
#1994=ADVANCED_FACE('',(#320),#1872,.F.);
#1995=ADVANCED_FACE('',(#321),#25,.T.);
#1996=ADVANCED_FACE('',(#322),#1873,.T.);
#1997=ADVANCED_FACE('',(#323),#1874,.F.);
#1998=ADVANCED_FACE('',(#324),#26,.T.);
#1999=ADVANCED_FACE('',(#325),#1875,.T.);
#2000=ADVANCED_FACE('',(#326),#1876,.F.);
#2001=ADVANCED_FACE('',(#327),#27,.T.);
#2002=ADVANCED_FACE('',(#328),#1877,.T.);
#2003=ADVANCED_FACE('',(#329),#1878,.F.);
#2004=ADVANCED_FACE('',(#330),#28,.T.);
#2005=ADVANCED_FACE('',(#331),#1879,.T.);
#2006=ADVANCED_FACE('',(#332),#1880,.F.);
#2007=ADVANCED_FACE('',(#333),#1881,.F.);
#2008=ADVANCED_FACE('',(#334),#1882,.F.);
#2009=ADVANCED_FACE('',(#335),#1883,.F.);
#2010=ADVANCED_FACE('',(#336),#1884,.F.);
#2011=ADVANCED_FACE('',(#337),#1885,.T.);
#2012=ADVANCED_FACE('',(#338),#1886,.F.);
#2013=ADVANCED_FACE('',(#339),#1887,.F.);
#2014=ADVANCED_FACE('',(#340),#1888,.F.);
#2015=ADVANCED_FACE('',(#341),#1889,.F.);
#2016=ADVANCED_FACE('',(#342),#1890,.F.);
#2017=ADVANCED_FACE('',(#343),#1891,.T.);
#2018=ADVANCED_FACE('',(#344),#1892,.F.);
#2019=ADVANCED_FACE('',(#345),#1893,.F.);
#2020=ADVANCED_FACE('',(#346),#1894,.F.);
#2021=ADVANCED_FACE('',(#347),#1895,.F.);
#2022=ADVANCED_FACE('',(#348),#1896,.F.);
#2023=ADVANCED_FACE('',(#349),#1897,.F.);
#2024=ADVANCED_FACE('',(#350),#1898,.T.);
#2025=CLOSED_SHELL('',(#1899,#1900,#1901,#1902,#1903,#1904));
#2026=CLOSED_SHELL('',(#1905,#1906,#1907,#1908,#1909,#1910));
#2027=CLOSED_SHELL('',(#1911,#1912,#1913,#1914,#1915,#1916));
#2028=CLOSED_SHELL('',(#1917,#1918,#1919,#1920,#1921,#1922));
#2029=CLOSED_SHELL('',(#1923,#1924,#1925));
#2030=CLOSED_SHELL('',(#1926,#1927,#1928,#1929,#1930,#1931));
#2031=CLOSED_SHELL('',(#1932,#1933,#1934,#1935,#1936,#1937));
#2032=CLOSED_SHELL('',(#1938,#1939,#1940,#1941,#1942,#1943));
#2033=CLOSED_SHELL('',(#1944,#1945,#1946,#1947,#1948,#1949));
#2034=CLOSED_SHELL('',(#1950,#1951,#1952,#1953,#1954,#1955));
#2035=CLOSED_SHELL('',(#1956,#1957,#1958,#1959,#1960,#1961));
#2036=CLOSED_SHELL('',(#1962,#1963,#1964));
#2037=CLOSED_SHELL('',(#1965,#1966,#1967,#1968,#1969,#1970));
#2038=CLOSED_SHELL('',(#1971,#1972,#1973,#1974,#1975,#1976));
#2039=CLOSED_SHELL('',(#1977,#1978,#1979,#1980,#1981,#1982));
#2040=CLOSED_SHELL('',(#1983,#1984,#1985,#1986,#1987,#1988));
#2041=CLOSED_SHELL('',(#1989,#1990,#1991,#1992,#1993,#1994));
#2042=CLOSED_SHELL('',(#1995,#1996,#1997));
#2043=CLOSED_SHELL('',(#1998,#1999,#2000));
#2044=CLOSED_SHELL('',(#2001,#2002,#2003));
#2045=CLOSED_SHELL('',(#2004,#2005,#2006));
#2046=CLOSED_SHELL('',(#2007,#2008,#2009,#2010,#2011,#2012));
#2047=CLOSED_SHELL('',(#2013,#2014,#2015,#2016,#2017,#2018));
#2048=CLOSED_SHELL('',(#2019,#2020,#2021,#2022,#2023,#2024));
#2049=DERIVED_UNIT_ELEMENT(#2097,1.);
#2050=DERIVED_UNIT_ELEMENT(#3727,-3.);
#2051=DERIVED_UNIT_ELEMENT(#2097,1.);
#2052=DERIVED_UNIT_ELEMENT(#3727,-3.);
#2053=DERIVED_UNIT_ELEMENT(#2097,1.);
#2054=DERIVED_UNIT_ELEMENT(#3727,-3.);
#2055=DERIVED_UNIT_ELEMENT(#2097,1.);
#2056=DERIVED_UNIT_ELEMENT(#3727,-3.);
#2057=DERIVED_UNIT_ELEMENT(#2097,1.);
#2058=DERIVED_UNIT_ELEMENT(#3727,-3.);
#2059=DERIVED_UNIT_ELEMENT(#2097,1.);
#2060=DERIVED_UNIT_ELEMENT(#3727,-3.);
#2061=DERIVED_UNIT_ELEMENT(#2097,1.);
#2062=DERIVED_UNIT_ELEMENT(#3727,-3.);
#2063=DERIVED_UNIT_ELEMENT(#2097,1.);
#2064=DERIVED_UNIT_ELEMENT(#3727,-3.);
#2065=DERIVED_UNIT_ELEMENT(#2097,1.);
#2066=DERIVED_UNIT_ELEMENT(#3727,-3.);
#2067=DERIVED_UNIT_ELEMENT(#2097,1.);
#2068=DERIVED_UNIT_ELEMENT(#3727,-3.);
#2069=DERIVED_UNIT_ELEMENT(#2097,1.);
#2070=DERIVED_UNIT_ELEMENT(#3727,-3.);
#2071=DERIVED_UNIT_ELEMENT(#2097,1.);
#2072=DERIVED_UNIT_ELEMENT(#3727,-3.);
#2073=DERIVED_UNIT_ELEMENT(#2097,1.);
#2074=DERIVED_UNIT_ELEMENT(#3727,-3.);
#2075=DERIVED_UNIT_ELEMENT(#2097,1.);
#2076=DERIVED_UNIT_ELEMENT(#3727,-3.);
#2077=DERIVED_UNIT_ELEMENT(#2097,1.);
#2078=DERIVED_UNIT_ELEMENT(#3727,-3.);
#2079=DERIVED_UNIT_ELEMENT(#2097,1.);
#2080=DERIVED_UNIT_ELEMENT(#3727,-3.);
#2081=DERIVED_UNIT_ELEMENT(#2097,1.);
#2082=DERIVED_UNIT_ELEMENT(#3727,-3.);
#2083=DERIVED_UNIT_ELEMENT(#2097,1.);
#2084=DERIVED_UNIT_ELEMENT(#3727,-3.);
#2085=DERIVED_UNIT_ELEMENT(#2097,1.);
#2086=DERIVED_UNIT_ELEMENT(#3727,-3.);
#2087=DERIVED_UNIT_ELEMENT(#2097,1.);
#2088=DERIVED_UNIT_ELEMENT(#3727,-3.);
#2089=DERIVED_UNIT_ELEMENT(#2097,1.);
#2090=DERIVED_UNIT_ELEMENT(#3727,-3.);
#2091=DERIVED_UNIT_ELEMENT(#2097,1.);
#2092=DERIVED_UNIT_ELEMENT(#3727,-3.);
#2093=DERIVED_UNIT_ELEMENT(#2097,1.);
#2094=DERIVED_UNIT_ELEMENT(#3727,-3.);
#2095=DERIVED_UNIT_ELEMENT(#2097,1.);
#2096=DERIVED_UNIT_ELEMENT(#3727,-3.);
#2097=(
MASS_UNIT()
NAMED_UNIT(*)
SI_UNIT(.KILO.,.GRAM.)
);
#2098=DERIVED_UNIT((#2049,#2050));
#2099=DERIVED_UNIT((#2051,#2052));
#2100=DERIVED_UNIT((#2053,#2054));
#2101=DERIVED_UNIT((#2055,#2056));
#2102=DERIVED_UNIT((#2057,#2058));
#2103=DERIVED_UNIT((#2059,#2060));
#2104=DERIVED_UNIT((#2061,#2062));
#2105=DERIVED_UNIT((#2063,#2064));
#2106=DERIVED_UNIT((#2065,#2066));
#2107=DERIVED_UNIT((#2067,#2068));
#2108=DERIVED_UNIT((#2069,#2070));
#2109=DERIVED_UNIT((#2071,#2072));
#2110=DERIVED_UNIT((#2073,#2074));
#2111=DERIVED_UNIT((#2075,#2076));
#2112=DERIVED_UNIT((#2077,#2078));
#2113=DERIVED_UNIT((#2079,#2080));
#2114=DERIVED_UNIT((#2081,#2082));
#2115=DERIVED_UNIT((#2083,#2084));
#2116=DERIVED_UNIT((#2085,#2086));
#2117=DERIVED_UNIT((#2087,#2088));
#2118=DERIVED_UNIT((#2089,#2090));
#2119=DERIVED_UNIT((#2091,#2092));
#2120=DERIVED_UNIT((#2093,#2094));
#2121=DERIVED_UNIT((#2095,#2096));
#2122=MEASURE_REPRESENTATION_ITEM('density measure',
POSITIVE_RATIO_MEASURE(630.),#2098);
#2123=MEASURE_REPRESENTATION_ITEM('density measure',
POSITIVE_RATIO_MEASURE(630.),#2099);
#2124=MEASURE_REPRESENTATION_ITEM('density measure',
POSITIVE_RATIO_MEASURE(630.),#2100);
#2125=MEASURE_REPRESENTATION_ITEM('density measure',
POSITIVE_RATIO_MEASURE(630.),#2101);
#2126=MEASURE_REPRESENTATION_ITEM('density measure',
POSITIVE_RATIO_MEASURE(630.),#2102);
#2127=MEASURE_REPRESENTATION_ITEM('density measure',
POSITIVE_RATIO_MEASURE(630.),#2103);
#2128=MEASURE_REPRESENTATION_ITEM('density measure',
POSITIVE_RATIO_MEASURE(630.),#2104);
#2129=MEASURE_REPRESENTATION_ITEM('density measure',
POSITIVE_RATIO_MEASURE(630.),#2105);
#2130=MEASURE_REPRESENTATION_ITEM('density measure',
POSITIVE_RATIO_MEASURE(630.),#2106);
#2131=MEASURE_REPRESENTATION_ITEM('density measure',
POSITIVE_RATIO_MEASURE(630.),#2107);
#2132=MEASURE_REPRESENTATION_ITEM('density measure',
POSITIVE_RATIO_MEASURE(630.),#2108);
#2133=MEASURE_REPRESENTATION_ITEM('density measure',
POSITIVE_RATIO_MEASURE(630.),#2109);
#2134=MEASURE_REPRESENTATION_ITEM('density measure',
POSITIVE_RATIO_MEASURE(630.),#2110);
#2135=MEASURE_REPRESENTATION_ITEM('density measure',
POSITIVE_RATIO_MEASURE(630.),#2111);
#2136=MEASURE_REPRESENTATION_ITEM('density measure',
POSITIVE_RATIO_MEASURE(630.),#2112);
#2137=MEASURE_REPRESENTATION_ITEM('density measure',
POSITIVE_RATIO_MEASURE(630.),#2113);
#2138=MEASURE_REPRESENTATION_ITEM('density measure',
POSITIVE_RATIO_MEASURE(630.),#2114);
#2139=MEASURE_REPRESENTATION_ITEM('density measure',
POSITIVE_RATIO_MEASURE(630.),#2115);
#2140=MEASURE_REPRESENTATION_ITEM('density measure',
POSITIVE_RATIO_MEASURE(630.),#2116);
#2141=MEASURE_REPRESENTATION_ITEM('density measure',
POSITIVE_RATIO_MEASURE(630.),#2117);
#2142=MEASURE_REPRESENTATION_ITEM('density measure',
POSITIVE_RATIO_MEASURE(630.),#2118);
#2143=MEASURE_REPRESENTATION_ITEM('density measure',
POSITIVE_RATIO_MEASURE(630.),#2119);
#2144=MEASURE_REPRESENTATION_ITEM('density measure',
POSITIVE_RATIO_MEASURE(630.),#2120);
#2145=MEASURE_REPRESENTATION_ITEM('density measure',
POSITIVE_RATIO_MEASURE(630.),#2121);
#2146=PROPERTY_DEFINITION_REPRESENTATION(#2266,#2194);
#2147=PROPERTY_DEFINITION_REPRESENTATION(#2267,#2195);
#2148=PROPERTY_DEFINITION_REPRESENTATION(#2268,#2196);
#2149=PROPERTY_DEFINITION_REPRESENTATION(#2269,#2197);
#2150=PROPERTY_DEFINITION_REPRESENTATION(#2270,#2198);
#2151=PROPERTY_DEFINITION_REPRESENTATION(#2271,#2199);
#2152=PROPERTY_DEFINITION_REPRESENTATION(#2272,#2200);
#2153=PROPERTY_DEFINITION_REPRESENTATION(#2273,#2201);
#2154=PROPERTY_DEFINITION_REPRESENTATION(#2274,#2202);
#2155=PROPERTY_DEFINITION_REPRESENTATION(#2275,#2203);
#2156=PROPERTY_DEFINITION_REPRESENTATION(#2276,#2204);
#2157=PROPERTY_DEFINITION_REPRESENTATION(#2277,#2205);
#2158=PROPERTY_DEFINITION_REPRESENTATION(#2278,#2206);
#2159=PROPERTY_DEFINITION_REPRESENTATION(#2279,#2207);
#2160=PROPERTY_DEFINITION_REPRESENTATION(#2280,#2208);
#2161=PROPERTY_DEFINITION_REPRESENTATION(#2281,#2209);
#2162=PROPERTY_DEFINITION_REPRESENTATION(#2282,#2210);
#2163=PROPERTY_DEFINITION_REPRESENTATION(#2283,#2211);
#2164=PROPERTY_DEFINITION_REPRESENTATION(#2284,#2212);
#2165=PROPERTY_DEFINITION_REPRESENTATION(#2285,#2213);
#2166=PROPERTY_DEFINITION_REPRESENTATION(#2286,#2214);
#2167=PROPERTY_DEFINITION_REPRESENTATION(#2287,#2215);
#2168=PROPERTY_DEFINITION_REPRESENTATION(#2288,#2216);
#2169=PROPERTY_DEFINITION_REPRESENTATION(#2289,#2217);
#2170=PROPERTY_DEFINITION_REPRESENTATION(#2290,#2218);
#2171=PROPERTY_DEFINITION_REPRESENTATION(#2291,#2219);
#2172=PROPERTY_DEFINITION_REPRESENTATION(#2292,#2220);
#2173=PROPERTY_DEFINITION_REPRESENTATION(#2293,#2221);
#2174=PROPERTY_DEFINITION_REPRESENTATION(#2294,#2222);
#2175=PROPERTY_DEFINITION_REPRESENTATION(#2295,#2223);
#2176=PROPERTY_DEFINITION_REPRESENTATION(#2296,#2224);
#2177=PROPERTY_DEFINITION_REPRESENTATION(#2297,#2225);
#2178=PROPERTY_DEFINITION_REPRESENTATION(#2298,#2226);
#2179=PROPERTY_DEFINITION_REPRESENTATION(#2299,#2227);
#2180=PROPERTY_DEFINITION_REPRESENTATION(#2300,#2228);
#2181=PROPERTY_DEFINITION_REPRESENTATION(#2301,#2229);
#2182=PROPERTY_DEFINITION_REPRESENTATION(#2302,#2230);
#2183=PROPERTY_DEFINITION_REPRESENTATION(#2303,#2231);
#2184=PROPERTY_DEFINITION_REPRESENTATION(#2304,#2232);
#2185=PROPERTY_DEFINITION_REPRESENTATION(#2305,#2233);
#2186=PROPERTY_DEFINITION_REPRESENTATION(#2306,#2234);
#2187=PROPERTY_DEFINITION_REPRESENTATION(#2307,#2235);
#2188=PROPERTY_DEFINITION_REPRESENTATION(#2308,#2236);
#2189=PROPERTY_DEFINITION_REPRESENTATION(#2309,#2237);
#2190=PROPERTY_DEFINITION_REPRESENTATION(#2310,#2238);
#2191=PROPERTY_DEFINITION_REPRESENTATION(#2311,#2239);
#2192=PROPERTY_DEFINITION_REPRESENTATION(#2312,#2240);
#2193=PROPERTY_DEFINITION_REPRESENTATION(#2313,#2241);
#2194=REPRESENTATION('material name',(#2242),#3699);
#2195=REPRESENTATION('density',(#2122),#3699);
#2196=REPRESENTATION('material name',(#2243),#3700);
#2197=REPRESENTATION('density',(#2123),#3700);
#2198=REPRESENTATION('material name',(#2244),#3701);
#2199=REPRESENTATION('density',(#2124),#3701);
#2200=REPRESENTATION('material name',(#2245),#3702);
#2201=REPRESENTATION('density',(#2125),#3702);
#2202=REPRESENTATION('material name',(#2246),#3703);
#2203=REPRESENTATION('density',(#2126),#3703);
#2204=REPRESENTATION('material name',(#2247),#3704);
#2205=REPRESENTATION('density',(#2127),#3704);
#2206=REPRESENTATION('material name',(#2248),#3705);
#2207=REPRESENTATION('density',(#2128),#3705);
#2208=REPRESENTATION('material name',(#2249),#3706);
#2209=REPRESENTATION('density',(#2129),#3706);
#2210=REPRESENTATION('material name',(#2250),#3707);
#2211=REPRESENTATION('density',(#2130),#3707);
#2212=REPRESENTATION('material name',(#2251),#3708);
#2213=REPRESENTATION('density',(#2131),#3708);
#2214=REPRESENTATION('material name',(#2252),#3709);
#2215=REPRESENTATION('density',(#2132),#3709);
#2216=REPRESENTATION('material name',(#2253),#3710);
#2217=REPRESENTATION('density',(#2133),#3710);
#2218=REPRESENTATION('material name',(#2254),#3711);
#2219=REPRESENTATION('density',(#2134),#3711);
#2220=REPRESENTATION('material name',(#2255),#3712);
#2221=REPRESENTATION('density',(#2135),#3712);
#2222=REPRESENTATION('material name',(#2256),#3713);
#2223=REPRESENTATION('density',(#2136),#3713);
#2224=REPRESENTATION('material name',(#2257),#3714);
#2225=REPRESENTATION('density',(#2137),#3714);
#2226=REPRESENTATION('material name',(#2258),#3715);
#2227=REPRESENTATION('density',(#2138),#3715);
#2228=REPRESENTATION('material name',(#2259),#3716);
#2229=REPRESENTATION('density',(#2139),#3716);
#2230=REPRESENTATION('material name',(#2260),#3717);
#2231=REPRESENTATION('density',(#2140),#3717);
#2232=REPRESENTATION('material name',(#2261),#3718);
#2233=REPRESENTATION('density',(#2141),#3718);
#2234=REPRESENTATION('material name',(#2262),#3719);
#2235=REPRESENTATION('density',(#2142),#3719);
#2236=REPRESENTATION('material name',(#2263),#3720);
#2237=REPRESENTATION('density',(#2143),#3720);
#2238=REPRESENTATION('material name',(#2264),#3721);
#2239=REPRESENTATION('density',(#2144),#3721);
#2240=REPRESENTATION('material name',(#2265),#3722);
#2241=REPRESENTATION('density',(#2145),#3722);
#2242=DESCRIPTIVE_REPRESENTATION_ITEM('Teak','Teak');
#2243=DESCRIPTIVE_REPRESENTATION_ITEM('Teak','Teak');
#2244=DESCRIPTIVE_REPRESENTATION_ITEM('Teak','Teak');
#2245=DESCRIPTIVE_REPRESENTATION_ITEM('Teak','Teak');
#2246=DESCRIPTIVE_REPRESENTATION_ITEM('Teak','Teak');
#2247=DESCRIPTIVE_REPRESENTATION_ITEM('Teak','Teak');
#2248=DESCRIPTIVE_REPRESENTATION_ITEM('Teak','Teak');
#2249=DESCRIPTIVE_REPRESENTATION_ITEM('Teak','Teak');
#2250=DESCRIPTIVE_REPRESENTATION_ITEM('Teak','Teak');
#2251=DESCRIPTIVE_REPRESENTATION_ITEM('Teak','Teak');
#2252=DESCRIPTIVE_REPRESENTATION_ITEM('Teak','Teak');
#2253=DESCRIPTIVE_REPRESENTATION_ITEM('Teak','Teak');
#2254=DESCRIPTIVE_REPRESENTATION_ITEM('Teak','Teak');
#2255=DESCRIPTIVE_REPRESENTATION_ITEM('Teak','Teak');
#2256=DESCRIPTIVE_REPRESENTATION_ITEM('Teak','Teak');
#2257=DESCRIPTIVE_REPRESENTATION_ITEM('Teak','Teak');
#2258=DESCRIPTIVE_REPRESENTATION_ITEM('Teak','Teak');
#2259=DESCRIPTIVE_REPRESENTATION_ITEM('Teak','Teak');
#2260=DESCRIPTIVE_REPRESENTATION_ITEM('Teak','Teak');
#2261=DESCRIPTIVE_REPRESENTATION_ITEM('Teak','Teak');
#2262=DESCRIPTIVE_REPRESENTATION_ITEM('Teak','Teak');
#2263=DESCRIPTIVE_REPRESENTATION_ITEM('Teak','Teak');
#2264=DESCRIPTIVE_REPRESENTATION_ITEM('Teak','Teak');
#2265=DESCRIPTIVE_REPRESENTATION_ITEM('Teak','Teak');
#2266=PROPERTY_DEFINITION('material property','material name',#3837);
#2267=PROPERTY_DEFINITION('material property','density of part',#3837);
#2268=PROPERTY_DEFINITION('material property','material name',#3838);
#2269=PROPERTY_DEFINITION('material property','density of part',#3838);
#2270=PROPERTY_DEFINITION('material property','material name',#3839);
#2271=PROPERTY_DEFINITION('material property','density of part',#3839);
#2272=PROPERTY_DEFINITION('material property','material name',#3840);
#2273=PROPERTY_DEFINITION('material property','density of part',#3840);
#2274=PROPERTY_DEFINITION('material property','material name',#3841);
#2275=PROPERTY_DEFINITION('material property','density of part',#3841);
#2276=PROPERTY_DEFINITION('material property','material name',#3842);
#2277=PROPERTY_DEFINITION('material property','density of part',#3842);
#2278=PROPERTY_DEFINITION('material property','material name',#3843);
#2279=PROPERTY_DEFINITION('material property','density of part',#3843);
#2280=PROPERTY_DEFINITION('material property','material name',#3844);
#2281=PROPERTY_DEFINITION('material property','density of part',#3844);
#2282=PROPERTY_DEFINITION('material property','material name',#3845);
#2283=PROPERTY_DEFINITION('material property','density of part',#3845);
#2284=PROPERTY_DEFINITION('material property','material name',#3846);
#2285=PROPERTY_DEFINITION('material property','density of part',#3846);
#2286=PROPERTY_DEFINITION('material property','material name',#3847);
#2287=PROPERTY_DEFINITION('material property','density of part',#3847);
#2288=PROPERTY_DEFINITION('material property','material name',#3848);
#2289=PROPERTY_DEFINITION('material property','density of part',#3848);
#2290=PROPERTY_DEFINITION('material property','material name',#3849);
#2291=PROPERTY_DEFINITION('material property','density of part',#3849);
#2292=PROPERTY_DEFINITION('material property','material name',#3850);
#2293=PROPERTY_DEFINITION('material property','density of part',#3850);
#2294=PROPERTY_DEFINITION('material property','material name',#3851);
#2295=PROPERTY_DEFINITION('material property','density of part',#3851);
#2296=PROPERTY_DEFINITION('material property','material name',#3852);
#2297=PROPERTY_DEFINITION('material property','density of part',#3852);
#2298=PROPERTY_DEFINITION('material property','material name',#3853);
#2299=PROPERTY_DEFINITION('material property','density of part',#3853);
#2300=PROPERTY_DEFINITION('material property','material name',#3854);
#2301=PROPERTY_DEFINITION('material property','density of part',#3854);
#2302=PROPERTY_DEFINITION('material property','material name',#3855);
#2303=PROPERTY_DEFINITION('material property','density of part',#3855);
#2304=PROPERTY_DEFINITION('material property','material name',#3856);
#2305=PROPERTY_DEFINITION('material property','density of part',#3856);
#2306=PROPERTY_DEFINITION('material property','material name',#3857);
#2307=PROPERTY_DEFINITION('material property','density of part',#3857);
#2308=PROPERTY_DEFINITION('material property','material name',#3858);
#2309=PROPERTY_DEFINITION('material property','density of part',#3858);
#2310=PROPERTY_DEFINITION('material property','material name',#3859);
#2311=PROPERTY_DEFINITION('material property','density of part',#3859);
#2312=PROPERTY_DEFINITION('material property','material name',#3860);
#2313=PROPERTY_DEFINITION('material property','density of part',#3860);
#2314=AXIS2_PLACEMENT_3D('',#3103,#2503,#2504);
#2315=AXIS2_PLACEMENT_3D('',#3104,#2505,#2506);
#2316=AXIS2_PLACEMENT_3D('',#3105,#2507,#2508);
#2317=AXIS2_PLACEMENT_3D('',#3106,#2509,#2510);
#2318=AXIS2_PLACEMENT_3D('',#3115,#2515,#2516);
#2319=AXIS2_PLACEMENT_3D('',#3121,#2520,#2521);
#2320=AXIS2_PLACEMENT_3D('',#3127,#2525,#2526);
#2321=AXIS2_PLACEMENT_3D('',#3130,#2529,#2530);
#2322=AXIS2_PLACEMENT_3D('',#3131,#2531,#2532);
#2323=AXIS2_PLACEMENT_3D('',#3132,#2533,#2534);
#2324=AXIS2_PLACEMENT_3D('',#3133,#2535,#2536);
#2325=AXIS2_PLACEMENT_3D('',#3134,#2537,#2538);
#2326=AXIS2_PLACEMENT_3D('',#3143,#2543,#2544);
#2327=AXIS2_PLACEMENT_3D('',#3149,#2548,#2549);
#2328=AXIS2_PLACEMENT_3D('',#3155,#2553,#2554);
#2329=AXIS2_PLACEMENT_3D('',#3158,#2557,#2558);
#2330=AXIS2_PLACEMENT_3D('',#3159,#2559,#2560);
#2331=AXIS2_PLACEMENT_3D('',#3160,#2561,#2562);
#2332=AXIS2_PLACEMENT_3D('',#3161,#2563,#2564);
#2333=AXIS2_PLACEMENT_3D('',#3170,#2569,#2570);
#2334=AXIS2_PLACEMENT_3D('',#3176,#2574,#2575);
#2335=AXIS2_PLACEMENT_3D('',#3182,#2579,#2580);
#2336=AXIS2_PLACEMENT_3D('',#3185,#2583,#2584);
#2337=AXIS2_PLACEMENT_3D('',#3186,#2585,#2586);
#2338=AXIS2_PLACEMENT_3D('',#3187,#2587,#2588);
#2339=AXIS2_PLACEMENT_3D('',#3188,#2589,#2590);
#2340=AXIS2_PLACEMENT_3D('',#3197,#2595,#2596);
#2341=AXIS2_PLACEMENT_3D('',#3203,#2600,#2601);
#2342=AXIS2_PLACEMENT_3D('',#3209,#2605,#2606);
#2343=AXIS2_PLACEMENT_3D('',#3212,#2609,#2610);
#2344=AXIS2_PLACEMENT_3D('',#3213,#2611,#2612);
#2345=AXIS2_PLACEMENT_3D('',#3214,#2613,#2614);
#2346=AXIS2_PLACEMENT_3D('',#3215,#2615,#2616);
#2347=AXIS2_PLACEMENT_3D('',#3217,#2617,#2618);
#2348=AXIS2_PLACEMENT_3D('',#3220,#2620,#2621);
#2349=AXIS2_PLACEMENT_3D('',#3221,#2622,#2623);
#2350=AXIS2_PLACEMENT_3D('',#3222,#2624,#2625);
#2351=AXIS2_PLACEMENT_3D('',#3223,#2626,#2627);
#2352=AXIS2_PLACEMENT_3D('',#3224,#2628,#2629);
#2353=AXIS2_PLACEMENT_3D('',#3233,#2634,#2635);
#2354=AXIS2_PLACEMENT_3D('',#3239,#2639,#2640);
#2355=AXIS2_PLACEMENT_3D('',#3245,#2644,#2645);
#2356=AXIS2_PLACEMENT_3D('',#3248,#2648,#2649);
#2357=AXIS2_PLACEMENT_3D('',#3249,#2650,#2651);
#2358=AXIS2_PLACEMENT_3D('',#3250,#2652,#2653);
#2359=AXIS2_PLACEMENT_3D('',#3251,#2654,#2655);
#2360=AXIS2_PLACEMENT_3D('',#3260,#2660,#2661);
#2361=AXIS2_PLACEMENT_3D('',#3266,#2665,#2666);
#2362=AXIS2_PLACEMENT_3D('',#3272,#2670,#2671);
#2363=AXIS2_PLACEMENT_3D('',#3275,#2674,#2675);
#2364=AXIS2_PLACEMENT_3D('',#3276,#2676,#2677);
#2365=AXIS2_PLACEMENT_3D('',#3277,#2678,#2679);
#2366=AXIS2_PLACEMENT_3D('',#3278,#2680,#2681);
#2367=AXIS2_PLACEMENT_3D('',#3287,#2686,#2687);
#2368=AXIS2_PLACEMENT_3D('',#3293,#2691,#2692);
#2369=AXIS2_PLACEMENT_3D('',#3299,#2696,#2697);
#2370=AXIS2_PLACEMENT_3D('',#3302,#2700,#2701);
#2371=AXIS2_PLACEMENT_3D('',#3303,#2702,#2703);
#2372=AXIS2_PLACEMENT_3D('',#3304,#2704,#2705);
#2373=AXIS2_PLACEMENT_3D('',#3305,#2706,#2707);
#2374=AXIS2_PLACEMENT_3D('',#3314,#2712,#2713);
#2375=AXIS2_PLACEMENT_3D('',#3320,#2717,#2718);
#2376=AXIS2_PLACEMENT_3D('',#3326,#2722,#2723);
#2377=AXIS2_PLACEMENT_3D('',#3329,#2726,#2727);
#2378=AXIS2_PLACEMENT_3D('',#3330,#2728,#2729);
#2379=AXIS2_PLACEMENT_3D('',#3331,#2730,#2731);
#2380=AXIS2_PLACEMENT_3D('',#3332,#2732,#2733);
#2381=AXIS2_PLACEMENT_3D('',#3341,#2738,#2739);
#2382=AXIS2_PLACEMENT_3D('',#3350,#2744,#2745);
#2383=AXIS2_PLACEMENT_3D('',#3353,#2748,#2749);
#2384=AXIS2_PLACEMENT_3D('',#3355,#2751,#2752);
#2385=AXIS2_PLACEMENT_3D('',#3357,#2754,#2755);
#2386=AXIS2_PLACEMENT_3D('',#3358,#2756,#2757);
#2387=AXIS2_PLACEMENT_3D('',#3359,#2758,#2759);
#2388=AXIS2_PLACEMENT_3D('',#3368,#2764,#2765);
#2389=AXIS2_PLACEMENT_3D('',#3374,#2769,#2770);
#2390=AXIS2_PLACEMENT_3D('',#3380,#2774,#2775);
#2391=AXIS2_PLACEMENT_3D('',#3383,#2778,#2779);
#2392=AXIS2_PLACEMENT_3D('',#3384,#2780,#2781);
#2393=AXIS2_PLACEMENT_3D('',#3385,#2782,#2783);
#2394=AXIS2_PLACEMENT_3D('',#3386,#2784,#2785);
#2395=AXIS2_PLACEMENT_3D('',#3388,#2786,#2787);
#2396=AXIS2_PLACEMENT_3D('',#3391,#2789,#2790);
#2397=AXIS2_PLACEMENT_3D('',#3392,#2791,#2792);
#2398=AXIS2_PLACEMENT_3D('',#3393,#2793,#2794);
#2399=AXIS2_PLACEMENT_3D('',#3394,#2795,#2796);
#2400=AXIS2_PLACEMENT_3D('',#3395,#2797,#2798);
#2401=AXIS2_PLACEMENT_3D('',#3404,#2803,#2804);
#2402=AXIS2_PLACEMENT_3D('',#3413,#2809,#2810);
#2403=AXIS2_PLACEMENT_3D('',#3416,#2813,#2814);
#2404=AXIS2_PLACEMENT_3D('',#3418,#2816,#2817);
#2405=AXIS2_PLACEMENT_3D('',#3420,#2819,#2820);
#2406=AXIS2_PLACEMENT_3D('',#3421,#2821,#2822);
#2407=AXIS2_PLACEMENT_3D('',#3422,#2823,#2824);
#2408=AXIS2_PLACEMENT_3D('',#3431,#2829,#2830);
#2409=AXIS2_PLACEMENT_3D('',#3437,#2834,#2835);
#2410=AXIS2_PLACEMENT_3D('',#3443,#2839,#2840);
#2411=AXIS2_PLACEMENT_3D('',#3446,#2843,#2844);
#2412=AXIS2_PLACEMENT_3D('',#3447,#2845,#2846);
#2413=AXIS2_PLACEMENT_3D('',#3448,#2847,#2848);
#2414=AXIS2_PLACEMENT_3D('',#3449,#2849,#2850);
#2415=AXIS2_PLACEMENT_3D('',#3458,#2855,#2856);
#2416=AXIS2_PLACEMENT_3D('',#3464,#2860,#2861);
#2417=AXIS2_PLACEMENT_3D('',#3470,#2865,#2866);
#2418=AXIS2_PLACEMENT_3D('',#3473,#2869,#2870);
#2419=AXIS2_PLACEMENT_3D('',#3474,#2871,#2872);
#2420=AXIS2_PLACEMENT_3D('',#3475,#2873,#2874);
#2421=AXIS2_PLACEMENT_3D('',#3476,#2875,#2876);
#2422=AXIS2_PLACEMENT_3D('',#3485,#2881,#2882);
#2423=AXIS2_PLACEMENT_3D('',#3491,#2886,#2887);
#2424=AXIS2_PLACEMENT_3D('',#3497,#2891,#2892);
#2425=AXIS2_PLACEMENT_3D('',#3500,#2895,#2896);
#2426=AXIS2_PLACEMENT_3D('',#3501,#2897,#2898);
#2427=AXIS2_PLACEMENT_3D('',#3502,#2899,#2900);
#2428=AXIS2_PLACEMENT_3D('',#3503,#2901,#2902);
#2429=AXIS2_PLACEMENT_3D('',#3512,#2907,#2908);
#2430=AXIS2_PLACEMENT_3D('',#3518,#2912,#2913);
#2431=AXIS2_PLACEMENT_3D('',#3524,#2917,#2918);
#2432=AXIS2_PLACEMENT_3D('',#3527,#2921,#2922);
#2433=AXIS2_PLACEMENT_3D('',#3528,#2923,#2924);
#2434=AXIS2_PLACEMENT_3D('',#3529,#2925,#2926);
#2435=AXIS2_PLACEMENT_3D('',#3530,#2927,#2928);
#2436=AXIS2_PLACEMENT_3D('',#3532,#2929,#2930);
#2437=AXIS2_PLACEMENT_3D('',#3535,#2932,#2933);
#2438=AXIS2_PLACEMENT_3D('',#3536,#2934,#2935);
#2439=AXIS2_PLACEMENT_3D('',#3537,#2936,#2937);
#2440=AXIS2_PLACEMENT_3D('',#3538,#2938,#2939);
#2441=AXIS2_PLACEMENT_3D('',#3539,#2940,#2941);
#2442=AXIS2_PLACEMENT_3D('',#3541,#2942,#2943);
#2443=AXIS2_PLACEMENT_3D('',#3544,#2945,#2946);
#2444=AXIS2_PLACEMENT_3D('',#3545,#2947,#2948);
#2445=AXIS2_PLACEMENT_3D('',#3546,#2949,#2950);
#2446=AXIS2_PLACEMENT_3D('',#3547,#2951,#2952);
#2447=AXIS2_PLACEMENT_3D('',#3548,#2953,#2954);
#2448=AXIS2_PLACEMENT_3D('',#3550,#2955,#2956);
#2449=AXIS2_PLACEMENT_3D('',#3553,#2958,#2959);
#2450=AXIS2_PLACEMENT_3D('',#3554,#2960,#2961);
#2451=AXIS2_PLACEMENT_3D('',#3555,#2962,#2963);
#2452=AXIS2_PLACEMENT_3D('',#3556,#2964,#2965);
#2453=AXIS2_PLACEMENT_3D('',#3557,#2966,#2967);
#2454=AXIS2_PLACEMENT_3D('',#3559,#2968,#2969);
#2455=AXIS2_PLACEMENT_3D('',#3562,#2971,#2972);
#2456=AXIS2_PLACEMENT_3D('',#3563,#2973,#2974);
#2457=AXIS2_PLACEMENT_3D('',#3564,#2975,#2976);
#2458=AXIS2_PLACEMENT_3D('',#3565,#2977,#2978);
#2459=AXIS2_PLACEMENT_3D('',#3566,#2979,#2980);
#2460=AXIS2_PLACEMENT_3D('',#3575,#2985,#2986);
#2461=AXIS2_PLACEMENT_3D('',#3581,#2990,#2991);
#2462=AXIS2_PLACEMENT_3D('',#3587,#2995,#2996);
#2463=AXIS2_PLACEMENT_3D('',#3590,#2999,#3000);
#2464=AXIS2_PLACEMENT_3D('',#3591,#3001,#3002);
#2465=AXIS2_PLACEMENT_3D('',#3592,#3003,#3004);
#2466=AXIS2_PLACEMENT_3D('',#3593,#3005,#3006);
#2467=AXIS2_PLACEMENT_3D('',#3602,#3011,#3012);
#2468=AXIS2_PLACEMENT_3D('',#3608,#3016,#3017);
#2469=AXIS2_PLACEMENT_3D('',#3614,#3021,#3022);
#2470=AXIS2_PLACEMENT_3D('',#3617,#3025,#3026);
#2471=AXIS2_PLACEMENT_3D('',#3618,#3027,#3028);
#2472=AXIS2_PLACEMENT_3D('',#3619,#3029,#3030);
#2473=AXIS2_PLACEMENT_3D('',#3620,#3031,#3032);
#2474=AXIS2_PLACEMENT_3D('',#3629,#3037,#3038);
#2475=AXIS2_PLACEMENT_3D('',#3635,#3042,#3043);
#2476=AXIS2_PLACEMENT_3D('',#3641,#3047,#3048);
#2477=AXIS2_PLACEMENT_3D('',#3644,#3051,#3052);
#2478=AXIS2_PLACEMENT_3D('',#3645,#3053,#3054);
#2479=AXIS2_PLACEMENT_3D('',#3646,#3055,#3056);
#2480=AXIS2_PLACEMENT_3D('',#3647,#3057,#3058);
#2481=AXIS2_PLACEMENT_3D('',#3648,#3059,#3060);
#2482=AXIS2_PLACEMENT_3D('',#3649,#3061,#3062);
#2483=AXIS2_PLACEMENT_3D('',#3650,#3063,#3064);
#2484=AXIS2_PLACEMENT_3D('',#3651,#3065,#3066);
#2485=AXIS2_PLACEMENT_3D('',#3652,#3067,#3068);
#2486=AXIS2_PLACEMENT_3D('',#3653,#3069,#3070);
#2487=AXIS2_PLACEMENT_3D('',#3654,#3071,#3072);
#2488=AXIS2_PLACEMENT_3D('',#3655,#3073,#3074);
#2489=AXIS2_PLACEMENT_3D('',#3656,#3075,#3076);
#2490=AXIS2_PLACEMENT_3D('',#3657,#3077,#3078);
#2491=AXIS2_PLACEMENT_3D('',#3658,#3079,#3080);
#2492=AXIS2_PLACEMENT_3D('',#3659,#3081,#3082);
#2493=AXIS2_PLACEMENT_3D('',#3660,#3083,#3084);
#2494=AXIS2_PLACEMENT_3D('',#3661,#3085,#3086);
#2495=AXIS2_PLACEMENT_3D('',#3662,#3087,#3088);
#2496=AXIS2_PLACEMENT_3D('',#3663,#3089,#3090);
#2497=AXIS2_PLACEMENT_3D('',#3664,#3091,#3092);
#2498=AXIS2_PLACEMENT_3D('',#3665,#3093,#3094);
#2499=AXIS2_PLACEMENT_3D('',#3666,#3095,#3096);
#2500=AXIS2_PLACEMENT_3D('',#3667,#3097,#3098);
#2501=AXIS2_PLACEMENT_3D('',#3668,#3099,#3100);
#2502=AXIS2_PLACEMENT_3D('',#3669,#3101,#3102);
#2503=DIRECTION('axis',(0.,0.,1.));
#2504=DIRECTION('refdir',(1.,0.,0.));
#2505=DIRECTION('axis',(0.,0.,1.));
#2506=DIRECTION('refdir',(1.,0.,0.));
#2507=DIRECTION('axis',(0.,0.,1.));
#2508=DIRECTION('refdir',(1.,0.,0.));
#2509=DIRECTION('center_axis',(-1.,-1.17112133399278E-16,0.));
#2510=DIRECTION('ref_axis',(0.,0.,1.));
#2511=DIRECTION('',(-1.49903530751076E-16,1.,0.));
#2512=DIRECTION('',(0.,0.,-1.));
#2513=DIRECTION('',(-1.49903530751076E-16,1.,0.));
#2514=DIRECTION('',(0.,0.,-1.));
#2515=DIRECTION('center_axis',(0.,-1.,0.));
#2516=DIRECTION('ref_axis',(0.,0.,-1.));
#2517=DIRECTION('',(-1.,0.,0.));
#2518=DIRECTION('',(0.,0.,-1.));
#2519=DIRECTION('',(-1.,0.,0.));
#2520=DIRECTION('center_axis',(1.,1.17112133399278E-16,0.));
#2521=DIRECTION('ref_axis',(0.,0.,-1.));
#2522=DIRECTION('',(1.49903530751076E-16,-1.,0.));
#2523=DIRECTION('',(0.,0.,-1.));
#2524=DIRECTION('',(1.49903530751076E-16,-1.,0.));
#2525=DIRECTION('center_axis',(0.,1.,0.));
#2526=DIRECTION('ref_axis',(0.,0.,1.));
#2527=DIRECTION('',(1.,0.,0.));
#2528=DIRECTION('',(1.,0.,0.));
#2529=DIRECTION('center_axis',(0.,0.,-1.));
#2530=DIRECTION('ref_axis',(-1.,0.,0.));
#2531=DIRECTION('center_axis',(0.,0.,-1.));
#2532=DIRECTION('ref_axis',(-1.,0.,0.));
#2533=DIRECTION('',(0.,0.,1.));
#2534=DIRECTION('',(1.,0.,0.));
#2535=DIRECTION('axis',(0.,0.,1.));
#2536=DIRECTION('refdir',(1.,0.,0.));
#2537=DIRECTION('center_axis',(1.,1.17112133399278E-16,0.));
#2538=DIRECTION('ref_axis',(0.,0.,-1.));
#2539=DIRECTION('',(1.49903530751076E-16,-1.,0.));
#2540=DIRECTION('',(0.,0.,-1.));
#2541=DIRECTION('',(1.49903530751076E-16,-1.,0.));
#2542=DIRECTION('',(0.,0.,-1.));
#2543=DIRECTION('center_axis',(0.,1.,0.));
#2544=DIRECTION('ref_axis',(0.,0.,1.));
#2545=DIRECTION('',(1.,0.,0.));
#2546=DIRECTION('',(0.,0.,-1.));
#2547=DIRECTION('',(1.,0.,0.));
#2548=DIRECTION('center_axis',(-1.,-1.17112133399278E-16,0.));
#2549=DIRECTION('ref_axis',(0.,0.,1.));
#2550=DIRECTION('',(-1.49903530751076E-16,1.,0.));
#2551=DIRECTION('',(0.,0.,-1.));
#2552=DIRECTION('',(-1.49903530751076E-16,1.,0.));
#2553=DIRECTION('center_axis',(0.,-1.,0.));
#2554=DIRECTION('ref_axis',(0.,0.,-1.));
#2555=DIRECTION('',(-1.,0.,0.));
#2556=DIRECTION('',(-1.,0.,0.));
#2557=DIRECTION('center_axis',(0.,0.,1.));
#2558=DIRECTION('ref_axis',(1.,0.,0.));
#2559=DIRECTION('center_axis',(0.,0.,1.));
#2560=DIRECTION('ref_axis',(1.,0.,0.));
#2561=DIRECTION('axis',(0.,0.,1.));
#2562=DIRECTION('refdir',(1.,0.,0.));
#2563=DIRECTION('center_axis',(1.,3.05589473088741E-16,0.));
#2564=DIRECTION('ref_axis',(0.,0.,-1.));
#2565=DIRECTION('',(3.05662668172116E-16,-1.,0.));
#2566=DIRECTION('',(0.,0.,-1.));
#2567=DIRECTION('',(3.05662668172116E-16,-1.,0.));
#2568=DIRECTION('',(0.,0.,-1.));
#2569=DIRECTION('center_axis',(0.,1.,0.));
#2570=DIRECTION('ref_axis',(0.,0.,1.));
#2571=DIRECTION('',(1.,0.,0.));
#2572=DIRECTION('',(0.,0.,-1.));
#2573=DIRECTION('',(1.,0.,0.));
#2574=DIRECTION('center_axis',(-1.,-3.05589473088741E-16,0.));
#2575=DIRECTION('ref_axis',(0.,0.,1.));
#2576=DIRECTION('',(-3.05662668172116E-16,1.,0.));
#2577=DIRECTION('',(0.,0.,-1.));
#2578=DIRECTION('',(-3.05662668172116E-16,1.,0.));
#2579=DIRECTION('center_axis',(0.,-1.,0.));
#2580=DIRECTION('ref_axis',(0.,0.,-1.));
#2581=DIRECTION('',(-1.,0.,0.));
#2582=DIRECTION('',(-1.,0.,0.));
#2583=DIRECTION('center_axis',(0.,0.,1.));
#2584=DIRECTION('ref_axis',(1.,0.,0.));
#2585=DIRECTION('center_axis',(0.,0.,1.));
#2586=DIRECTION('ref_axis',(1.,0.,0.));
#2587=DIRECTION('axis',(0.,0.,1.));
#2588=DIRECTION('refdir',(1.,0.,0.));
#2589=DIRECTION('center_axis',(-1.,0.,0.));
#2590=DIRECTION('ref_axis',(0.,0.,1.));
#2591=DIRECTION('',(0.,1.,0.));
#2592=DIRECTION('',(0.,0.,-1.));
#2593=DIRECTION('',(0.,1.,0.));
#2594=DIRECTION('',(0.,0.,-1.));
#2595=DIRECTION('center_axis',(0.,-1.,0.));
#2596=DIRECTION('ref_axis',(0.,0.,-1.));
#2597=DIRECTION('',(-1.,0.,0.));
#2598=DIRECTION('',(-1.,0.,0.));
#2599=DIRECTION('',(0.,0.,-1.));
#2600=DIRECTION('center_axis',(1.,0.,0.));
#2601=DIRECTION('ref_axis',(0.,0.,-1.));
#2602=DIRECTION('',(0.,-1.,0.));
#2603=DIRECTION('',(0.,-1.,0.));
#2604=DIRECTION('',(0.,0.,-1.));
#2605=DIRECTION('center_axis',(0.,1.,0.));
#2606=DIRECTION('ref_axis',(0.,0.,1.));
#2607=DIRECTION('',(1.,0.,0.));
#2608=DIRECTION('',(1.,0.,0.));
#2609=DIRECTION('center_axis',(0.,0.,1.));
#2610=DIRECTION('ref_axis',(1.,0.,0.));
#2611=DIRECTION('center_axis',(0.,0.,1.));
#2612=DIRECTION('ref_axis',(1.,0.,0.));
#2613=DIRECTION('axis',(0.,0.,1.));
#2614=DIRECTION('refdir',(1.,0.,0.));
#2615=DIRECTION('center_axis',(0.,1.,0.));
#2616=DIRECTION('ref_axis',(0.,0.,1.));
#2617=DIRECTION('center_axis',(0.,-1.,0.));
#2618=DIRECTION('ref_axis',(0.,0.,-1.));
#2619=DIRECTION('',(0.,-1.,0.));
#2620=DIRECTION('center_axis',(0.,-1.,0.));
#2621=DIRECTION('ref_axis',(0.,0.,-1.));
#2622=DIRECTION('center_axis',(0.,-1.,0.));
#2623=DIRECTION('ref_axis',(0.,0.,-1.));
#2624=DIRECTION('center_axis',(0.,-1.,0.));
#2625=DIRECTION('ref_axis',(0.,0.,-1.));
#2626=DIRECTION('axis',(0.,0.,1.));
#2627=DIRECTION('refdir',(1.,0.,0.));
#2628=DIRECTION('center_axis',(-1.,0.,0.));
#2629=DIRECTION('ref_axis',(0.,0.,1.));
#2630=DIRECTION('',(0.,0.,-1.));
#2631=DIRECTION('',(0.,1.,0.));
#2632=DIRECTION('',(0.,0.,-1.));
#2633=DIRECTION('',(0.,1.,0.));
#2634=DIRECTION('center_axis',(0.,1.,0.));
#2635=DIRECTION('ref_axis',(0.,0.,1.));
#2636=DIRECTION('',(1.,0.,0.));
#2637=DIRECTION('',(1.,0.,0.));
#2638=DIRECTION('',(0.,0.,-1.));
#2639=DIRECTION('center_axis',(-1.,0.,0.));
#2640=DIRECTION('ref_axis',(0.,0.,1.));
#2641=DIRECTION('',(0.,1.,0.));
#2642=DIRECTION('',(0.,1.,0.));
#2643=DIRECTION('',(0.,0.,-1.));
#2644=DIRECTION('center_axis',(0.,-1.,0.));
#2645=DIRECTION('ref_axis',(0.,0.,-1.));
#2646=DIRECTION('',(-1.,0.,0.));
#2647=DIRECTION('',(-1.,0.,0.));
#2648=DIRECTION('center_axis',(0.,0.,1.));
#2649=DIRECTION('ref_axis',(1.,0.,0.));
#2650=DIRECTION('center_axis',(0.,0.,1.));
#2651=DIRECTION('ref_axis',(1.,0.,0.));
#2652=DIRECTION('axis',(0.,0.,1.));
#2653=DIRECTION('refdir',(1.,0.,0.));
#2654=DIRECTION('center_axis',(1.,0.,0.));
#2655=DIRECTION('ref_axis',(0.,0.,-1.));
#2656=DIRECTION('',(0.,-1.,0.));
#2657=DIRECTION('',(0.,0.,-1.));
#2658=DIRECTION('',(0.,-1.,0.));
#2659=DIRECTION('',(0.,0.,-1.));
#2660=DIRECTION('center_axis',(0.,1.,0.));
#2661=DIRECTION('ref_axis',(0.,0.,1.));
#2662=DIRECTION('',(1.,0.,0.));
#2663=DIRECTION('',(0.,0.,-1.));
#2664=DIRECTION('',(1.,0.,0.));
#2665=DIRECTION('center_axis',(1.,0.,0.));
#2666=DIRECTION('ref_axis',(0.,0.,-1.));
#2667=DIRECTION('',(0.,-1.,0.));
#2668=DIRECTION('',(0.,0.,-1.));
#2669=DIRECTION('',(0.,-1.,0.));
#2670=DIRECTION('center_axis',(0.,1.,0.));
#2671=DIRECTION('ref_axis',(0.,0.,1.));
#2672=DIRECTION('',(1.,0.,0.));
#2673=DIRECTION('',(1.,0.,0.));
#2674=DIRECTION('center_axis',(0.,0.,1.));
#2675=DIRECTION('ref_axis',(1.,0.,0.));
#2676=DIRECTION('center_axis',(0.,0.,1.));
#2677=DIRECTION('ref_axis',(1.,0.,0.));
#2678=DIRECTION('axis',(0.,0.,1.));
#2679=DIRECTION('refdir',(1.,0.,0.));
#2680=DIRECTION('center_axis',(-1.,0.,0.));
#2681=DIRECTION('ref_axis',(0.,0.,1.));
#2682=DIRECTION('',(0.,1.,0.));
#2683=DIRECTION('',(0.,0.,-1.));
#2684=DIRECTION('',(0.,1.,0.));
#2685=DIRECTION('',(0.,0.,-1.));
#2686=DIRECTION('center_axis',(-7.50657893593751E-16,-1.,0.));
#2687=DIRECTION('ref_axis',(0.,0.,-1.));
#2688=DIRECTION('',(-1.,9.60842103800001E-16,0.));
#2689=DIRECTION('',(-1.,9.60842103800001E-16,0.));
#2690=DIRECTION('',(0.,0.,-1.));
#2691=DIRECTION('center_axis',(1.,0.,0.));
#2692=DIRECTION('ref_axis',(0.,0.,-1.));
#2693=DIRECTION('',(0.,-1.,0.));
#2694=DIRECTION('',(0.,-1.,0.));
#2695=DIRECTION('',(0.,0.,-1.));
#2696=DIRECTION('center_axis',(0.,1.,0.));
#2697=DIRECTION('ref_axis',(0.,0.,1.));
#2698=DIRECTION('',(1.,0.,0.));
#2699=DIRECTION('',(1.,0.,0.));
#2700=DIRECTION('center_axis',(0.,0.,1.));
#2701=DIRECTION('ref_axis',(1.,0.,0.));
#2702=DIRECTION('center_axis',(0.,0.,1.));
#2703=DIRECTION('ref_axis',(1.,0.,0.));
#2704=DIRECTION('axis',(0.,0.,1.));
#2705=DIRECTION('refdir',(1.,0.,0.));
#2706=DIRECTION('center_axis',(1.,1.19276216655045E-16,0.));
#2707=DIRECTION('ref_axis',(0.,0.,-1.));
#2708=DIRECTION('',(1.52673557318457E-16,-1.,0.));
#2709=DIRECTION('',(0.,0.,-1.));
#2710=DIRECTION('',(1.52673557318457E-16,-1.,0.));
#2711=DIRECTION('',(0.,0.,-1.));
#2712=DIRECTION('center_axis',(0.,1.,0.));
#2713=DIRECTION('ref_axis',(0.,0.,1.));
#2714=DIRECTION('',(1.,0.,0.));
#2715=DIRECTION('',(1.,0.,0.));
#2716=DIRECTION('',(0.,0.,-1.));
#2717=DIRECTION('center_axis',(-1.,-1.19276216655045E-16,0.));
#2718=DIRECTION('ref_axis',(0.,0.,1.));
#2719=DIRECTION('',(-1.52673557318457E-16,1.,0.));
#2720=DIRECTION('',(-1.52673557318457E-16,1.,0.));
#2721=DIRECTION('',(0.,0.,-1.));
#2722=DIRECTION('center_axis',(0.,-1.,0.));
#2723=DIRECTION('ref_axis',(0.,0.,-1.));
#2724=DIRECTION('',(-1.,0.,0.));
#2725=DIRECTION('',(-1.,0.,0.));
#2726=DIRECTION('center_axis',(0.,0.,1.));
#2727=DIRECTION('ref_axis',(1.,0.,0.));
#2728=DIRECTION('center_axis',(0.,0.,1.));
#2729=DIRECTION('ref_axis',(1.,0.,0.));
#2730=DIRECTION('axis',(0.,0.,1.));
#2731=DIRECTION('refdir',(1.,0.,0.));
#2732=DIRECTION('center_axis',(0.,0.,1.));
#2733=DIRECTION('ref_axis',(1.,0.,0.));
#2734=DIRECTION('',(1.,0.,0.));
#2735=DIRECTION('',(0.,-1.,0.));
#2736=DIRECTION('',(1.,0.,0.));
#2737=DIRECTION('',(0.,-1.,0.));
#2738=DIRECTION('center_axis',(0.,0.,1.));
#2739=DIRECTION('ref_axis',(1.,0.,0.));
#2740=DIRECTION('',(0.,-1.,0.));
#2741=DIRECTION('',(1.,0.,0.));
#2742=DIRECTION('',(0.,-1.,0.));
#2743=DIRECTION('',(1.,0.,0.));
#2744=DIRECTION('center_axis',(0.,1.,0.));
#2745=DIRECTION('ref_axis',(0.,0.,1.));
#2746=DIRECTION('',(0.,0.,-1.));
#2747=DIRECTION('',(0.,0.,-1.));
#2748=DIRECTION('center_axis',(1.,0.,0.));
#2749=DIRECTION('ref_axis',(0.,0.,-1.));
#2750=DIRECTION('',(0.,0.,-1.));
#2751=DIRECTION('center_axis',(0.,1.,0.));
#2752=DIRECTION('ref_axis',(0.,0.,1.));
#2753=DIRECTION('',(0.,0.,-1.));
#2754=DIRECTION('center_axis',(1.,0.,0.));
#2755=DIRECTION('ref_axis',(0.,0.,-1.));
#2756=DIRECTION('axis',(0.,0.,1.));
#2757=DIRECTION('refdir',(1.,0.,0.));
#2758=DIRECTION('center_axis',(-1.,0.,0.));
#2759=DIRECTION('ref_axis',(0.,0.,1.));
#2760=DIRECTION('',(0.,0.,-1.));
#2761=DIRECTION('',(0.,1.,0.));
#2762=DIRECTION('',(0.,0.,-1.));
#2763=DIRECTION('',(0.,1.,0.));
#2764=DIRECTION('center_axis',(0.,-1.,0.));
#2765=DIRECTION('ref_axis',(0.,0.,-1.));
#2766=DIRECTION('',(0.,0.,-1.));
#2767=DIRECTION('',(-1.,0.,0.));
#2768=DIRECTION('',(-1.,0.,0.));
#2769=DIRECTION('center_axis',(-1.,0.,0.));
#2770=DIRECTION('ref_axis',(0.,0.,1.));
#2771=DIRECTION('',(0.,1.,0.));
#2772=DIRECTION('',(0.,1.,0.));
#2773=DIRECTION('',(0.,0.,-1.));
#2774=DIRECTION('center_axis',(0.,-1.,0.));
#2775=DIRECTION('ref_axis',(0.,0.,-1.));
#2776=DIRECTION('',(-1.,0.,0.));
#2777=DIRECTION('',(-1.,0.,0.));
#2778=DIRECTION('center_axis',(0.,0.,1.));
#2779=DIRECTION('ref_axis',(1.,0.,0.));
#2780=DIRECTION('center_axis',(0.,0.,1.));
#2781=DIRECTION('ref_axis',(1.,0.,0.));
#2782=DIRECTION('axis',(0.,0.,1.));
#2783=DIRECTION('refdir',(1.,0.,0.));
#2784=DIRECTION('center_axis',(0.,1.,0.));
#2785=DIRECTION('ref_axis',(0.,0.,1.));
#2786=DIRECTION('center_axis',(0.,-1.,0.));
#2787=DIRECTION('ref_axis',(0.,0.,-1.));
#2788=DIRECTION('',(0.,-1.,0.));
#2789=DIRECTION('center_axis',(0.,-1.,0.));
#2790=DIRECTION('ref_axis',(0.,0.,-1.));
#2791=DIRECTION('center_axis',(0.,-1.,0.));
#2792=DIRECTION('ref_axis',(0.,0.,-1.));
#2793=DIRECTION('center_axis',(0.,-1.,0.));
#2794=DIRECTION('ref_axis',(0.,0.,-1.));
#2795=DIRECTION('axis',(0.,0.,1.));
#2796=DIRECTION('refdir',(1.,0.,0.));
#2797=DIRECTION('center_axis',(0.,0.,1.));
#2798=DIRECTION('ref_axis',(1.,0.,0.));
#2799=DIRECTION('',(1.,0.,0.));
#2800=DIRECTION('',(0.,-1.,0.));
#2801=DIRECTION('',(1.,0.,0.));
#2802=DIRECTION('',(0.,-1.,0.));
#2803=DIRECTION('center_axis',(0.,0.,1.));
#2804=DIRECTION('ref_axis',(1.,0.,0.));
#2805=DIRECTION('',(0.,-1.,0.));
#2806=DIRECTION('',(1.,0.,0.));
#2807=DIRECTION('',(0.,-1.,0.));
#2808=DIRECTION('',(1.,0.,0.));
#2809=DIRECTION('center_axis',(0.,1.,0.));
#2810=DIRECTION('ref_axis',(0.,0.,1.));
#2811=DIRECTION('',(0.,0.,-1.));
#2812=DIRECTION('',(0.,0.,-1.));
#2813=DIRECTION('center_axis',(1.,0.,0.));
#2814=DIRECTION('ref_axis',(0.,0.,-1.));
#2815=DIRECTION('',(0.,0.,-1.));
#2816=DIRECTION('center_axis',(0.,1.,0.));
#2817=DIRECTION('ref_axis',(0.,0.,1.));
#2818=DIRECTION('',(0.,0.,-1.));
#2819=DIRECTION('center_axis',(1.,0.,0.));
#2820=DIRECTION('ref_axis',(0.,0.,-1.));
#2821=DIRECTION('axis',(0.,0.,1.));
#2822=DIRECTION('refdir',(1.,0.,0.));
#2823=DIRECTION('center_axis',(1.,1.17112133399278E-16,0.));
#2824=DIRECTION('ref_axis',(0.,0.,-1.));
#2825=DIRECTION('',(0.,-1.,0.));
#2826=DIRECTION('',(0.,0.,-1.));
#2827=DIRECTION('',(0.,-1.,0.));
#2828=DIRECTION('',(0.,0.,-1.));
#2829=DIRECTION('center_axis',(0.,1.,0.));
#2830=DIRECTION('ref_axis',(0.,0.,1.));
#2831=DIRECTION('',(1.,0.,0.));
#2832=DIRECTION('',(0.,0.,-1.));
#2833=DIRECTION('',(1.,0.,0.));
#2834=DIRECTION('center_axis',(-1.,-9.88133625556409E-17,0.));
#2835=DIRECTION('ref_axis',(0.,0.,1.));
#2836=DIRECTION('',(-1.23358113847239E-16,1.,0.));
#2837=DIRECTION('',(0.,0.,-1.));
#2838=DIRECTION('',(-1.23358113847239E-16,1.,0.));
#2839=DIRECTION('center_axis',(0.,1.,0.));
#2840=DIRECTION('ref_axis',(0.,0.,1.));
#2841=DIRECTION('',(1.,0.,0.));
#2842=DIRECTION('',(1.,0.,0.));
#2843=DIRECTION('center_axis',(0.,0.,1.));
#2844=DIRECTION('ref_axis',(1.,0.,0.));
#2845=DIRECTION('center_axis',(0.,0.,1.));
#2846=DIRECTION('ref_axis',(1.,0.,0.));
#2847=DIRECTION('axis',(0.,0.,1.));
#2848=DIRECTION('refdir',(1.,0.,0.));
#2849=DIRECTION('center_axis',(-1.,0.,0.));
#2850=DIRECTION('ref_axis',(0.,0.,1.));
#2851=DIRECTION('',(0.,1.,0.));
#2852=DIRECTION('',(0.,0.,-1.));
#2853=DIRECTION('',(0.,1.,0.));
#2854=DIRECTION('',(0.,0.,-1.));
#2855=DIRECTION('center_axis',(-7.50657893593751E-16,-1.,0.));
#2856=DIRECTION('ref_axis',(0.,0.,-1.));
#2857=DIRECTION('',(-1.,9.60842103800001E-16,0.));
#2858=DIRECTION('',(-1.,9.60842103800001E-16,0.));
#2859=DIRECTION('',(0.,0.,-1.));
#2860=DIRECTION('center_axis',(1.,0.,0.));
#2861=DIRECTION('ref_axis',(0.,0.,-1.));
#2862=DIRECTION('',(0.,-1.,0.));
#2863=DIRECTION('',(0.,-1.,0.));
#2864=DIRECTION('',(0.,0.,-1.));
#2865=DIRECTION('center_axis',(0.,1.,0.));
#2866=DIRECTION('ref_axis',(0.,0.,1.));
#2867=DIRECTION('',(1.,0.,0.));
#2868=DIRECTION('',(1.,0.,0.));
#2869=DIRECTION('center_axis',(0.,0.,1.));
#2870=DIRECTION('ref_axis',(1.,0.,0.));
#2871=DIRECTION('center_axis',(0.,0.,1.));
#2872=DIRECTION('ref_axis',(1.,0.,0.));
#2873=DIRECTION('axis',(0.,0.,1.));
#2874=DIRECTION('refdir',(1.,0.,0.));
#2875=DIRECTION('center_axis',(1.,5.24779270478898E-17,0.));
#2876=DIRECTION('ref_axis',(0.,0.,-1.));
#2877=DIRECTION('',(6.71717466212989E-17,-1.,0.));
#2878=DIRECTION('',(0.,0.,-1.));
#2879=DIRECTION('',(6.71717466212989E-17,-1.,0.));
#2880=DIRECTION('',(0.,0.,-1.));
#2881=DIRECTION('center_axis',(0.,1.,0.));
#2882=DIRECTION('ref_axis',(0.,0.,1.));
#2883=DIRECTION('',(1.,0.,0.));
#2884=DIRECTION('',(1.,0.,0.));
#2885=DIRECTION('',(0.,0.,-1.));
#2886=DIRECTION('center_axis',(-1.,-1.0495585409578E-16,0.));
#2887=DIRECTION('ref_axis',(0.,0.,1.));
#2888=DIRECTION('',(-1.00757619931948E-16,1.,0.));
#2889=DIRECTION('',(-1.00757619931948E-16,1.,0.));
#2890=DIRECTION('',(0.,0.,-1.));
#2891=DIRECTION('center_axis',(0.,-1.,0.));
#2892=DIRECTION('ref_axis',(0.,0.,-1.));
#2893=DIRECTION('',(-1.,0.,0.));
#2894=DIRECTION('',(-1.,0.,0.));
#2895=DIRECTION('center_axis',(0.,0.,1.));
#2896=DIRECTION('ref_axis',(1.,0.,0.));
#2897=DIRECTION('center_axis',(0.,0.,1.));
#2898=DIRECTION('ref_axis',(1.,0.,0.));
#2899=DIRECTION('axis',(0.,0.,1.));
#2900=DIRECTION('refdir',(1.,0.,0.));
#2901=DIRECTION('center_axis',(1.,-1.85037170770859E-14,-1.98679854084674E-16));
#2902=DIRECTION('ref_axis',(-1.98679854084674E-16,0.,-1.));
#2903=DIRECTION('',(0.,0.,1.));
#2904=DIRECTION('',(-2.36847578586702E-14,-1.,0.));
#2905=DIRECTION('',(2.54310213228382E-16,0.,1.));
#2906=DIRECTION('',(-1.57898385724468E-14,-1.,-2.04540917754051E-46));
#2907=DIRECTION('center_axis',(3.77483350043889E-60,2.04540917754051E-46,
-1.));
#2908=DIRECTION('ref_axis',(-1.,0.,-3.77483350043889E-60));
#2909=DIRECTION('',(1.,-1.84940038397751E-14,0.));
#2910=DIRECTION('',(-1.57898385724468E-14,-1.,0.));
#2911=DIRECTION('',(1.,-1.84940038397751E-14,0.));
#2912=DIRECTION('center_axis',(-1.,1.85037170770859E-14,0.));
#2913=DIRECTION('ref_axis',(0.,0.,1.));
#2914=DIRECTION('',(0.,0.,-1.));
#2915=DIRECTION('',(-1.57898385724468E-14,-1.,-2.04540917754051E-46));
#2916=DIRECTION('',(0.,0.,-1.));
#2917=DIRECTION('center_axis',(9.93377236957248E-63,-2.04540917754051E-46,
1.));
#2918=DIRECTION('ref_axis',(1.,0.,-9.93377236957248E-63));
#2919=DIRECTION('',(-1.,1.84940038397751E-14,3.78476727280846E-60));
#2920=DIRECTION('',(-1.,1.84940038397751E-14,3.78432352684346E-60));
#2921=DIRECTION('center_axis',(1.84551508905319E-14,1.,-3.66666668604152E-30));
#2922=DIRECTION('ref_axis',(0.,3.66666668604152E-30,1.));
#2923=DIRECTION('center_axis',(1.84551508905319E-14,1.,-3.66666668604152E-30));
#2924=DIRECTION('ref_axis',(0.,3.66666668604152E-30,1.));
#2925=DIRECTION('axis',(0.,0.,1.));
#2926=DIRECTION('refdir',(1.,0.,0.));
#2927=DIRECTION('center_axis',(0.,1.,0.));
#2928=DIRECTION('ref_axis',(0.,0.,1.));
#2929=DIRECTION('center_axis',(0.,-1.,0.));
#2930=DIRECTION('ref_axis',(0.,0.,-1.));
#2931=DIRECTION('',(0.,-1.,0.));
#2932=DIRECTION('center_axis',(0.,-1.,0.));
#2933=DIRECTION('ref_axis',(0.,0.,-1.));
#2934=DIRECTION('center_axis',(0.,-1.,0.));
#2935=DIRECTION('ref_axis',(0.,0.,-1.));
#2936=DIRECTION('center_axis',(0.,-1.,0.));
#2937=DIRECTION('ref_axis',(0.,0.,-1.));
#2938=DIRECTION('axis',(0.,0.,1.));
#2939=DIRECTION('refdir',(1.,0.,0.));
#2940=DIRECTION('center_axis',(0.,1.,0.));
#2941=DIRECTION('ref_axis',(0.,0.,1.));
#2942=DIRECTION('center_axis',(0.,-1.,0.));
#2943=DIRECTION('ref_axis',(0.,0.,-1.));
#2944=DIRECTION('',(0.,-1.,0.));
#2945=DIRECTION('center_axis',(0.,-1.,0.));
#2946=DIRECTION('ref_axis',(0.,0.,-1.));
#2947=DIRECTION('center_axis',(0.,-1.,0.));
#2948=DIRECTION('ref_axis',(0.,0.,-1.));
#2949=DIRECTION('center_axis',(0.,-1.,0.));
#2950=DIRECTION('ref_axis',(0.,0.,-1.));
#2951=DIRECTION('axis',(0.,0.,1.));
#2952=DIRECTION('refdir',(1.,0.,0.));
#2953=DIRECTION('center_axis',(0.,1.,0.));
#2954=DIRECTION('ref_axis',(0.,0.,1.));
#2955=DIRECTION('center_axis',(0.,-1.,0.));
#2956=DIRECTION('ref_axis',(0.,0.,-1.));
#2957=DIRECTION('',(0.,-1.,0.));
#2958=DIRECTION('center_axis',(0.,-1.,0.));
#2959=DIRECTION('ref_axis',(0.,0.,-1.));
#2960=DIRECTION('center_axis',(0.,-1.,0.));
#2961=DIRECTION('ref_axis',(0.,0.,-1.));
#2962=DIRECTION('center_axis',(0.,-1.,0.));
#2963=DIRECTION('ref_axis',(0.,0.,-1.));
#2964=DIRECTION('axis',(0.,0.,1.));
#2965=DIRECTION('refdir',(1.,0.,0.));
#2966=DIRECTION('center_axis',(0.,1.,0.));
#2967=DIRECTION('ref_axis',(0.,0.,1.));
#2968=DIRECTION('center_axis',(0.,-1.,0.));
#2969=DIRECTION('ref_axis',(0.,0.,-1.));
#2970=DIRECTION('',(0.,-1.,0.));
#2971=DIRECTION('center_axis',(0.,-1.,0.));
#2972=DIRECTION('ref_axis',(0.,0.,-1.));
#2973=DIRECTION('center_axis',(0.,-1.,0.));
#2974=DIRECTION('ref_axis',(0.,0.,-1.));
#2975=DIRECTION('center_axis',(0.,-1.,0.));
#2976=DIRECTION('ref_axis',(0.,0.,-1.));
#2977=DIRECTION('axis',(0.,0.,1.));
#2978=DIRECTION('refdir',(1.,0.,0.));
#2979=DIRECTION('center_axis',(1.,1.17112133399278E-16,0.));
#2980=DIRECTION('ref_axis',(0.,0.,-1.));
#2981=DIRECTION('',(1.49903530751076E-16,-1.,0.));
#2982=DIRECTION('',(0.,0.,-1.));
#2983=DIRECTION('',(1.49903530751076E-16,-1.,0.));
#2984=DIRECTION('',(0.,0.,-1.));
#2985=DIRECTION('center_axis',(0.,1.,0.));
#2986=DIRECTION('ref_axis',(0.,0.,1.));
#2987=DIRECTION('',(1.,0.,0.));
#2988=DIRECTION('',(0.,0.,-1.));
#2989=DIRECTION('',(1.,0.,0.));
#2990=DIRECTION('center_axis',(-1.,-9.88133625556409E-17,0.));
#2991=DIRECTION('ref_axis',(0.,0.,1.));
#2992=DIRECTION('',(-9.895975272239E-17,1.,0.));
#2993=DIRECTION('',(0.,0.,-1.));
#2994=DIRECTION('',(-9.895975272239E-17,1.,0.));
#2995=DIRECTION('center_axis',(0.,-1.,0.));
#2996=DIRECTION('ref_axis',(0.,0.,-1.));
#2997=DIRECTION('',(-1.,0.,0.));
#2998=DIRECTION('',(-1.,0.,0.));
#2999=DIRECTION('center_axis',(0.,0.,1.));
#3000=DIRECTION('ref_axis',(1.,0.,0.));
#3001=DIRECTION('center_axis',(0.,0.,1.));
#3002=DIRECTION('ref_axis',(1.,0.,0.));
#3003=DIRECTION('axis',(0.,0.,1.));
#3004=DIRECTION('refdir',(1.,0.,0.));
#3005=DIRECTION('center_axis',(1.,0.,1.98679854084674E-16));
#3006=DIRECTION('ref_axis',(1.98679854084674E-16,0.,-1.));
#3007=DIRECTION('',(2.54310213228382E-16,0.,-1.));
#3008=DIRECTION('',(0.,1.,0.));
#3009=DIRECTION('',(2.54310213228382E-16,0.,-1.));
#3010=DIRECTION('',(0.,1.,0.));
#3011=DIRECTION('center_axis',(0.,0.,1.));
#3012=DIRECTION('ref_axis',(1.,0.,0.));
#3013=DIRECTION('',(1.,0.,0.));
#3014=DIRECTION('',(0.,1.,0.));
#3015=DIRECTION('',(1.,0.,0.));
#3016=DIRECTION('center_axis',(-1.,0.,-3.97359708169347E-16));
#3017=DIRECTION('ref_axis',(-3.97359708169347E-16,0.,1.));
#3018=DIRECTION('',(-2.54310213228382E-16,0.,1.));
#3019=DIRECTION('',(0.,1.,0.));
#3020=DIRECTION('',(-2.54310213228382E-16,0.,1.));
#3021=DIRECTION('center_axis',(0.,0.,-1.));
#3022=DIRECTION('ref_axis',(-1.,0.,0.));
#3023=DIRECTION('',(-1.,0.,0.));
#3024=DIRECTION('',(-1.,0.,0.));
#3025=DIRECTION('center_axis',(0.,-1.,0.));
#3026=DIRECTION('ref_axis',(0.,0.,-1.));
#3027=DIRECTION('center_axis',(0.,-1.,0.));
#3028=DIRECTION('ref_axis',(0.,0.,-1.));
#3029=DIRECTION('axis',(0.,0.,1.));
#3030=DIRECTION('refdir',(1.,0.,0.));
#3031=DIRECTION('center_axis',(1.,0.,0.));
#3032=DIRECTION('ref_axis',(0.,0.,-1.));
#3033=DIRECTION('',(0.,-1.,0.));
#3034=DIRECTION('',(0.,0.,-1.));
#3035=DIRECTION('',(0.,-1.,0.));
#3036=DIRECTION('',(0.,0.,-1.));
#3037=DIRECTION('center_axis',(0.,1.,0.));
#3038=DIRECTION('ref_axis',(0.,0.,1.));
#3039=DIRECTION('',(1.,0.,0.));
#3040=DIRECTION('',(0.,0.,-1.));
#3041=DIRECTION('',(1.,0.,0.));
#3042=DIRECTION('center_axis',(-1.,0.,0.));
#3043=DIRECTION('ref_axis',(0.,0.,1.));
#3044=DIRECTION('',(0.,1.,0.));
#3045=DIRECTION('',(0.,0.,-1.));
#3046=DIRECTION('',(0.,1.,0.));
#3047=DIRECTION('center_axis',(0.,-1.,0.));
#3048=DIRECTION('ref_axis',(0.,0.,-1.));
#3049=DIRECTION('',(-1.,0.,0.));
#3050=DIRECTION('',(-1.,0.,0.));
#3051=DIRECTION('center_axis',(0.,0.,-1.));
#3052=DIRECTION('ref_axis',(-1.,0.,0.));
#3053=DIRECTION('center_axis',(0.,0.,-1.));
#3054=DIRECTION('ref_axis',(-1.,0.,0.));
#3055=DIRECTION('',(0.,0.,1.));
#3056=DIRECTION('',(1.,0.,0.));
#3057=DIRECTION('',(0.,0.,1.));
#3058=DIRECTION('',(1.,0.,0.));
#3059=DIRECTION('',(0.,0.,1.));
#3060=DIRECTION('',(1.,0.,0.));
#3061=DIRECTION('',(0.,0.,1.));
#3062=DIRECTION('',(1.,0.,0.));
#3063=DIRECTION('',(0.,0.,1.));
#3064=DIRECTION('',(1.,0.,0.));
#3065=DIRECTION('',(0.,0.,1.));
#3066=DIRECTION('',(1.,0.,0.));
#3067=DIRECTION('',(0.,0.,1.));
#3068=DIRECTION('',(1.,0.,0.));
#3069=DIRECTION('',(0.,0.,1.));
#3070=DIRECTION('',(1.,0.,0.));
#3071=DIRECTION('',(0.,0.,1.));
#3072=DIRECTION('',(1.,0.,0.));
#3073=DIRECTION('',(0.,0.,1.));
#3074=DIRECTION('',(1.,0.,0.));
#3075=DIRECTION('',(0.,0.,1.));
#3076=DIRECTION('',(1.,0.,0.));
#3077=DIRECTION('',(0.,0.,1.));
#3078=DIRECTION('',(1.,0.,0.));
#3079=DIRECTION('',(0.,0.,1.));
#3080=DIRECTION('',(1.,0.,0.));
#3081=DIRECTION('',(0.,0.,1.));
#3082=DIRECTION('',(1.,0.,0.));
#3083=DIRECTION('',(0.,0.,1.));
#3084=DIRECTION('',(1.,0.,0.));
#3085=DIRECTION('',(0.,0.,1.));
#3086=DIRECTION('',(1.,0.,0.));
#3087=DIRECTION('',(0.,0.,1.));
#3088=DIRECTION('',(1.,0.,0.));
#3089=DIRECTION('',(0.,0.,1.));
#3090=DIRECTION('',(1.,0.,0.));
#3091=DIRECTION('',(0.,0.,1.));
#3092=DIRECTION('',(1.,0.,0.));
#3093=DIRECTION('',(0.,0.,1.));
#3094=DIRECTION('',(1.,0.,0.));
#3095=DIRECTION('',(0.,0.,1.));
#3096=DIRECTION('',(1.,0.,0.));
#3097=DIRECTION('',(0.,0.,1.));
#3098=DIRECTION('',(1.,0.,0.));
#3099=DIRECTION('',(0.,0.,1.));
#3100=DIRECTION('',(1.,0.,0.));
#3101=DIRECTION('',(0.,0.,1.));
#3102=DIRECTION('',(1.,0.,0.));
#3103=CARTESIAN_POINT('',(0.,0.,0.));
#3104=CARTESIAN_POINT('',(0.,0.,0.));
#3105=CARTESIAN_POINT('',(0.,0.,0.));
#3106=CARTESIAN_POINT('Origin',(36.,79.2913385826772,22.));
#3107=CARTESIAN_POINT('',(36.,4.64566929133859,0.));
#3108=CARTESIAN_POINT('',(36.,79.2913385826772,0.));
#3109=CARTESIAN_POINT('',(36.,4.64566929133859,0.));
#3110=CARTESIAN_POINT('',(36.,79.2913385826772,22.));
#3111=CARTESIAN_POINT('',(36.,79.2913385826772,22.));
#3112=CARTESIAN_POINT('',(36.,4.64566929133859,22.));
#3113=CARTESIAN_POINT('',(36.,4.64566929133859,22.));
#3114=CARTESIAN_POINT('',(36.,4.64566929133859,22.));
#3115=CARTESIAN_POINT('Origin',(36.,79.2913385826772,22.));
#3116=CARTESIAN_POINT('',(35.2913385826772,79.2913385826772,0.));
#3117=CARTESIAN_POINT('',(36.,79.2913385826772,0.));
#3118=CARTESIAN_POINT('',(35.2913385826772,79.2913385826772,22.));
#3119=CARTESIAN_POINT('',(35.2913385826772,79.2913385826772,22.));
#3120=CARTESIAN_POINT('',(36.,79.2913385826772,22.));
#3121=CARTESIAN_POINT('Origin',(35.2913385826772,79.2913385826772,22.));
#3122=CARTESIAN_POINT('',(35.2913385826772,4.64566929133859,0.));
#3123=CARTESIAN_POINT('',(35.2913385826772,79.2913385826772,0.));
#3124=CARTESIAN_POINT('',(35.2913385826772,4.64566929133859,22.));
#3125=CARTESIAN_POINT('',(35.2913385826772,4.64566929133859,22.));
#3126=CARTESIAN_POINT('',(35.2913385826772,79.2913385826772,22.));
#3127=CARTESIAN_POINT('Origin',(36.,4.64566929133859,22.));
#3128=CARTESIAN_POINT('',(35.2913385826772,4.64566929133859,0.));
#3129=CARTESIAN_POINT('',(35.2913385826772,4.64566929133859,22.));
#3130=CARTESIAN_POINT('Origin',(0.,0.,22.));
#3131=CARTESIAN_POINT('Origin',(0.,0.,0.));
#3132=CARTESIAN_POINT('',(0.,0.,0.));
#3133=CARTESIAN_POINT('',(0.,0.,0.));
#3134=CARTESIAN_POINT('Origin',(-36.,79.2913385826772,22.));
#3135=CARTESIAN_POINT('',(-36.,79.2913385826772,0.));
#3136=CARTESIAN_POINT('',(-36.,4.64566929133858,0.));
#3137=CARTESIAN_POINT('',(-36.,79.2913385826772,0.));
#3138=CARTESIAN_POINT('',(-36.,4.64566929133858,22.));
#3139=CARTESIAN_POINT('',(-36.,4.64566929133858,22.));
#3140=CARTESIAN_POINT('',(-36.,79.2913385826772,22.));
#3141=CARTESIAN_POINT('',(-36.,79.2913385826772,22.));
#3142=CARTESIAN_POINT('',(-36.,79.2913385826772,22.));
#3143=CARTESIAN_POINT('Origin',(-36.,4.64566929133858,22.));
#3144=CARTESIAN_POINT('',(-35.2913385826772,4.64566929133858,0.));
#3145=CARTESIAN_POINT('',(-36.,4.64566929133858,0.));
#3146=CARTESIAN_POINT('',(-35.2913385826772,4.64566929133858,22.));
#3147=CARTESIAN_POINT('',(-35.2913385826772,4.64566929133858,22.));
#3148=CARTESIAN_POINT('',(-36.,4.64566929133858,22.));
#3149=CARTESIAN_POINT('Origin',(-35.2913385826772,79.2913385826772,22.));
#3150=CARTESIAN_POINT('',(-35.2913385826772,79.2913385826772,0.));
#3151=CARTESIAN_POINT('',(-35.2913385826772,4.64566929133858,0.));
#3152=CARTESIAN_POINT('',(-35.2913385826772,79.2913385826772,22.));
#3153=CARTESIAN_POINT('',(-35.2913385826772,79.2913385826772,22.));
#3154=CARTESIAN_POINT('',(-35.2913385826772,4.64566929133858,22.));
#3155=CARTESIAN_POINT('Origin',(-36.,79.2913385826772,22.));
#3156=CARTESIAN_POINT('',(-35.2913385826772,79.2913385826772,0.));
#3157=CARTESIAN_POINT('',(-35.2913385826772,79.2913385826772,22.));
#3158=CARTESIAN_POINT('Origin',(0.,0.,22.));
#3159=CARTESIAN_POINT('Origin',(0.,0.,0.));
#3160=CARTESIAN_POINT('',(0.,0.,0.));
#3161=CARTESIAN_POINT('Origin',(-0.354330708661419,4.64566929133858,22.));
#3162=CARTESIAN_POINT('',(-0.354330708661442,79.2913385826772,0.));
#3163=CARTESIAN_POINT('',(-0.354330708661419,4.64566929133858,0.));
#3164=CARTESIAN_POINT('',(-0.354330708661442,79.2913385826772,0.));
#3165=CARTESIAN_POINT('',(-0.354330708661419,4.64566929133858,22.));
#3166=CARTESIAN_POINT('',(-0.354330708661419,4.64566929133858,22.));
#3167=CARTESIAN_POINT('',(-0.354330708661442,79.2913385826772,22.));
#3168=CARTESIAN_POINT('',(-0.354330708661442,79.2913385826772,22.));
#3169=CARTESIAN_POINT('',(-0.354330708661442,79.2913385826772,22.));
#3170=CARTESIAN_POINT('Origin',(0.354330708661416,4.64566929133858,22.));
#3171=CARTESIAN_POINT('',(0.354330708661416,4.64566929133858,0.));
#3172=CARTESIAN_POINT('',(-0.354330708661419,4.64566929133858,0.));
#3173=CARTESIAN_POINT('',(0.354330708661416,4.64566929133858,22.));
#3174=CARTESIAN_POINT('',(0.354330708661416,4.64566929133858,22.));
#3175=CARTESIAN_POINT('',(-0.354330708661419,4.64566929133858,22.));
#3176=CARTESIAN_POINT('Origin',(0.354330708661416,4.64566929133858,22.));
#3177=CARTESIAN_POINT('',(0.354330708661393,79.2913385826772,0.));
#3178=CARTESIAN_POINT('',(0.354330708661416,4.64566929133858,0.));
#3179=CARTESIAN_POINT('',(0.354330708661393,79.2913385826772,22.));
#3180=CARTESIAN_POINT('',(0.354330708661393,79.2913385826772,22.));
#3181=CARTESIAN_POINT('',(0.354330708661416,4.64566929133858,22.));
#3182=CARTESIAN_POINT('Origin',(0.354330708661393,79.2913385826772,22.));
#3183=CARTESIAN_POINT('',(0.354330708661393,79.2913385826772,0.));
#3184=CARTESIAN_POINT('',(0.354330708661393,79.2913385826772,22.));
#3185=CARTESIAN_POINT('Origin',(0.,0.,22.));
#3186=CARTESIAN_POINT('Origin',(0.,0.,0.));
#3187=CARTESIAN_POINT('',(0.,0.,0.));
#3188=CARTESIAN_POINT('Origin',(-0.354330708661442,39.3359580052493,30.375872491424));
#3189=CARTESIAN_POINT('',(-0.354330708661442,38.6272965879265,18.7086614173228));
#3190=CARTESIAN_POINT('',(-0.354330708661442,39.3359580052493,18.7086614173228));
#3191=CARTESIAN_POINT('',(-0.354330708661442,38.6272965879265,18.7086614173228));
#3192=CARTESIAN_POINT('',(-0.354330708661442,38.6272965879265,0.708661417322834));
#3193=CARTESIAN_POINT('',(-0.354330708661442,38.6272965879265,18.7086614173228));
#3194=CARTESIAN_POINT('',(-0.354330708661442,39.3359580052493,0.708661417322834));
#3195=CARTESIAN_POINT('',(-0.354330708661442,38.6272965879265,0.708661417322834));
#3196=CARTESIAN_POINT('',(-0.354330708661442,39.3359580052493,18.7086614173228));
#3197=CARTESIAN_POINT('Origin',(-12.,39.3359580052493,30.375872491424));
#3198=CARTESIAN_POINT('',(-12.,39.3359580052493,18.7086614173228));
#3199=CARTESIAN_POINT('',(-0.354330708661442,39.3359580052493,18.7086614173228));
#3200=CARTESIAN_POINT('',(-12.,39.3359580052493,0.708661417322834));
#3201=CARTESIAN_POINT('',(-0.354330708661446,39.3359580052493,0.708661417322834));
#3202=CARTESIAN_POINT('',(-12.,39.3359580052493,18.7086614173228));
#3203=CARTESIAN_POINT('Origin',(-12.,39.3359580052493,30.375872491424));
#3204=CARTESIAN_POINT('',(-12.,38.6272965879265,18.7086614173228));
#3205=CARTESIAN_POINT('',(-12.,39.3359580052493,18.7086614173228));
#3206=CARTESIAN_POINT('',(-12.,38.6272965879265,0.708661417322834));
#3207=CARTESIAN_POINT('',(-12.,39.3359580052493,0.708661417322834));
#3208=CARTESIAN_POINT('',(-12.,38.6272965879265,18.7086614173228));
#3209=CARTESIAN_POINT('Origin',(-12.,38.6272965879265,30.375872491424));
#3210=CARTESIAN_POINT('',(-12.,38.6272965879265,18.7086614173228));
#3211=CARTESIAN_POINT('',(-12.,38.6272965879265,0.708661417322834));
#3212=CARTESIAN_POINT('Origin',(0.,0.,0.708661417322834));
#3213=CARTESIAN_POINT('Origin',(0.,0.,18.7086614173228));
#3214=CARTESIAN_POINT('',(0.,0.,0.));
#3215=CARTESIAN_POINT('Origin',(8.74191357972564E-15,-4.91732638859567E-15,
19.6377952755906));
#3216=CARTESIAN_POINT('',(8.74191357972564E-15,3.93700787401574,17.6692913385827));
#3217=CARTESIAN_POINT('Origin',(8.74191357972564E-15,3.93700787401574,19.6377952755906));
#3218=CARTESIAN_POINT('',(8.74191357972564E-15,-4.91732638859567E-15,17.6692913385827));
#3219=CARTESIAN_POINT('',(8.50084137516908E-15,-4.91732638859567E-15,17.6692913385827));
#3220=CARTESIAN_POINT('Origin',(8.74191357972564E-15,-4.91732638859567E-15,
19.6377952755906));
#3221=CARTESIAN_POINT('Origin',(8.74191357972564E-15,-4.91732638859567E-15,
19.6377952755906));
#3222=CARTESIAN_POINT('Origin',(8.74191357972564E-15,3.93700787401574,19.6377952755906));
#3223=CARTESIAN_POINT('',(0.,0.,0.));
#3224=CARTESIAN_POINT('Origin',(-12.7086614173228,0.,46.6558556092144));
#3225=CARTESIAN_POINT('',(-12.7086614173228,4.64566929133858,22.));
#3226=CARTESIAN_POINT('',(-12.7086614173228,4.64566929133858,0.708661417322834));
#3227=CARTESIAN_POINT('',(-12.7086614173228,4.64566929133858,22.));
#3228=CARTESIAN_POINT('',(-12.7086614173228,24.2913385826772,22.));
#3229=CARTESIAN_POINT('',(-12.7086614173228,4.64566929133858,22.));
#3230=CARTESIAN_POINT('',(-12.7086614173228,24.2913385826772,0.708661417322834));
#3231=CARTESIAN_POINT('',(-12.7086614173228,24.2913385826772,22.));
#3232=CARTESIAN_POINT('',(-12.7086614173228,4.64566929133858,0.708661417322834));
#3233=CARTESIAN_POINT('Origin',(0.,4.64566929133858,46.6558556092144));
#3234=CARTESIAN_POINT('',(-12.,4.64566929133858,22.));
#3235=CARTESIAN_POINT('',(-12.7086614173228,4.64566929133858,22.));
#3236=CARTESIAN_POINT('',(-12.,4.64566929133858,0.708661417322834));
#3237=CARTESIAN_POINT('',(-12.7086614173228,4.64566929133858,0.708661417322834));
#3238=CARTESIAN_POINT('',(-12.,4.64566929133858,22.));
#3239=CARTESIAN_POINT('Origin',(-12.,0.,46.6558556092144));
#3240=CARTESIAN_POINT('',(-12.,24.2913385826772,22.));
#3241=CARTESIAN_POINT('',(-12.,4.64566929133858,22.));
#3242=CARTESIAN_POINT('',(-12.,24.2913385826772,0.708661417322834));
#3243=CARTESIAN_POINT('',(-12.,4.64566929133858,0.708661417322834));
#3244=CARTESIAN_POINT('',(-12.,24.2913385826772,22.));
#3245=CARTESIAN_POINT('Origin',(0.,24.2913385826772,46.6558556092144));
#3246=CARTESIAN_POINT('',(-12.,24.2913385826772,22.));
#3247=CARTESIAN_POINT('',(-12.,24.2913385826772,0.708661417322834));
#3248=CARTESIAN_POINT('Origin',(0.,0.,0.708661417322834));
#3249=CARTESIAN_POINT('Origin',(0.,0.,22.));
#3250=CARTESIAN_POINT('',(0.,0.,0.));
#3251=CARTESIAN_POINT('Origin',(35.2913385826772,0.,18.7086614173228));
#3252=CARTESIAN_POINT('',(35.2913385826772,67.3543307086614,0.708661417322834));
#3253=CARTESIAN_POINT('',(35.2913385826772,66.6456692913386,0.708661417322834));
#3254=CARTESIAN_POINT('',(35.2913385826772,67.3543307086614,0.708661417322834));
#3255=CARTESIAN_POINT('',(35.2913385826772,67.3543307086614,18.7086614173228));
#3256=CARTESIAN_POINT('',(35.2913385826772,67.3543307086614,18.7086614173228));
#3257=CARTESIAN_POINT('',(35.2913385826772,66.6456692913386,18.7086614173228));
#3258=CARTESIAN_POINT('',(35.2913385826772,67.3543307086614,18.7086614173228));
#3259=CARTESIAN_POINT('',(35.2913385826772,66.6456692913386,18.7086614173228));
#3260=CARTESIAN_POINT('Origin',(0.,67.3543307086614,18.7086614173228));
#3261=CARTESIAN_POINT('',(0.354330708661416,67.3543307086614,0.708661417322834));
#3262=CARTESIAN_POINT('',(0.354330708661416,67.3543307086614,0.708661417322834));
#3263=CARTESIAN_POINT('',(0.354330708661416,67.3543307086614,18.7086614173228));
#3264=CARTESIAN_POINT('',(0.354330708661416,67.3543307086614,18.7086614173228));
#3265=CARTESIAN_POINT('',(0.354330708661416,67.3543307086614,18.7086614173228));
#3266=CARTESIAN_POINT('Origin',(0.354330708661416,0.,18.7086614173228));
#3267=CARTESIAN_POINT('',(0.354330708661416,66.6456692913386,0.708661417322834));
#3268=CARTESIAN_POINT('',(0.354330708661416,67.3543307086614,0.708661417322834));
#3269=CARTESIAN_POINT('',(0.354330708661416,66.6456692913386,18.7086614173228));
#3270=CARTESIAN_POINT('',(0.354330708661416,66.6456692913386,18.7086614173228));
#3271=CARTESIAN_POINT('',(0.354330708661416,67.3543307086614,18.7086614173228));
#3272=CARTESIAN_POINT('Origin',(0.,66.6456692913386,18.7086614173228));
#3273=CARTESIAN_POINT('',(0.354330708661416,66.6456692913386,0.708661417322834));
#3274=CARTESIAN_POINT('',(0.354330708661416,66.6456692913386,18.7086614173228));
#3275=CARTESIAN_POINT('Origin',(0.,0.,18.7086614173228));
#3276=CARTESIAN_POINT('Origin',(0.,0.,0.708661417322834));
#3277=CARTESIAN_POINT('',(0.,0.,0.));
#3278=CARTESIAN_POINT('Origin',(-0.354330708661419,53.1679790026247,30.375872491424));
#3279=CARTESIAN_POINT('',(-0.354330708661418,52.4593175853018,18.7086614173228));
#3280=CARTESIAN_POINT('',(-0.354330708661419,53.1679790026247,18.7086614173228));
#3281=CARTESIAN_POINT('',(-0.354330708661419,52.4593175853018,18.7086614173228));
#3282=CARTESIAN_POINT('',(-0.354330708661419,52.4593175853018,0.708661417322834));
#3283=CARTESIAN_POINT('',(-0.354330708661419,52.4593175853018,18.7086614173228));
#3284=CARTESIAN_POINT('',(-0.354330708661419,53.1679790026247,0.708661417322834));
#3285=CARTESIAN_POINT('',(-0.354330708661419,52.4593175853018,0.708661417322834));
#3286=CARTESIAN_POINT('',(-0.354330708661419,53.1679790026247,18.7086614173228));
#3287=CARTESIAN_POINT('Origin',(-12.,53.1679790026247,30.375872491424));
#3288=CARTESIAN_POINT('',(-12.,53.1679790026247,18.7086614173228));
#3289=CARTESIAN_POINT('',(-0.35433070866142,53.1679790026247,18.7086614173228));
#3290=CARTESIAN_POINT('',(-12.,53.1679790026247,0.708661417322834));
#3291=CARTESIAN_POINT('',(-0.35433070866142,53.1679790026247,0.708661417322834));
#3292=CARTESIAN_POINT('',(-12.,53.1679790026247,18.7086614173228));
#3293=CARTESIAN_POINT('Origin',(-12.,53.1679790026247,30.375872491424));
#3294=CARTESIAN_POINT('',(-12.,52.4593175853018,18.7086614173228));
#3295=CARTESIAN_POINT('',(-12.,53.1679790026247,18.7086614173228));
#3296=CARTESIAN_POINT('',(-12.,52.4593175853018,0.708661417322834));
#3297=CARTESIAN_POINT('',(-12.,53.1679790026247,0.708661417322834));
#3298=CARTESIAN_POINT('',(-12.,52.4593175853018,18.7086614173228));
#3299=CARTESIAN_POINT('Origin',(-12.,52.4593175853018,30.375872491424));
#3300=CARTESIAN_POINT('',(-12.,52.4593175853018,18.7086614173228));
#3301=CARTESIAN_POINT('',(-12.,52.4593175853018,0.708661417322834));
#3302=CARTESIAN_POINT('Origin',(0.,0.,0.708661417322834));
#3303=CARTESIAN_POINT('Origin',(0.,0.,18.7086614173228));
#3304=CARTESIAN_POINT('',(0.,0.,0.));
#3305=CARTESIAN_POINT('Origin',(22.9370078740157,66.6456692913386,60.3603597227694));
#3306=CARTESIAN_POINT('',(22.9370078740157,66.6456692913386,18.7086614173228));
#3307=CARTESIAN_POINT('',(22.9370078740157,30.,18.7086614173228));
#3308=CARTESIAN_POINT('',(22.9370078740157,66.6456692913386,18.7086614173228));
#3309=CARTESIAN_POINT('',(22.9370078740157,66.6456692913386,0.708661417322834));
#3310=CARTESIAN_POINT('',(22.9370078740157,66.6456692913386,18.7086614173228));
#3311=CARTESIAN_POINT('',(22.9370078740157,30.,0.708661417322834));
#3312=CARTESIAN_POINT('',(22.9370078740157,66.6456692913386,0.708661417322834));
#3313=CARTESIAN_POINT('',(22.9370078740157,30.,18.7086614173228));
#3314=CARTESIAN_POINT('Origin',(22.9370078740157,30.,60.3603597227694));
#3315=CARTESIAN_POINT('',(23.6456692913386,30.,18.7086614173228));
#3316=CARTESIAN_POINT('',(22.9370078740157,30.,18.7086614173228));
#3317=CARTESIAN_POINT('',(23.6456692913386,30.,0.708661417322834));
#3318=CARTESIAN_POINT('',(22.9370078740157,30.,0.708661417322834));
#3319=CARTESIAN_POINT('',(23.6456692913386,30.,18.7086614173228));
#3320=CARTESIAN_POINT('Origin',(23.6456692913386,66.6456692913386,60.3603597227694));
#3321=CARTESIAN_POINT('',(23.6456692913386,66.6456692913386,18.7086614173228));
#3322=CARTESIAN_POINT('',(23.6456692913386,30.,18.7086614173228));
#3323=CARTESIAN_POINT('',(23.6456692913386,66.6456692913386,0.708661417322834));
#3324=CARTESIAN_POINT('',(23.6456692913386,30.,0.708661417322834));
#3325=CARTESIAN_POINT('',(23.6456692913386,66.6456692913386,18.7086614173228));
#3326=CARTESIAN_POINT('Origin',(22.9370078740157,66.6456692913386,60.3603597227694));
#3327=CARTESIAN_POINT('',(23.6456692913386,66.6456692913386,18.7086614173228));
#3328=CARTESIAN_POINT('',(23.6456692913386,66.6456692913386,0.708661417322834));
#3329=CARTESIAN_POINT('Origin',(0.,0.,0.708661417322834));
#3330=CARTESIAN_POINT('Origin',(0.,0.,18.7086614173228));
#3331=CARTESIAN_POINT('',(0.,0.,0.));
#3332=CARTESIAN_POINT('Origin',(0.,0.,22.));
#3333=CARTESIAN_POINT('',(-35.2913385826772,25.,22.));
#3334=CARTESIAN_POINT('',(-0.354330708661419,25.,22.));
#3335=CARTESIAN_POINT('',(-35.2913385826772,25.,22.));
#3336=CARTESIAN_POINT('',(-35.2913385826772,24.2913385826772,22.));
#3337=CARTESIAN_POINT('',(-35.2913385826772,25.,22.));
#3338=CARTESIAN_POINT('',(-0.354330708661419,24.2913385826772,22.));
#3339=CARTESIAN_POINT('',(-35.2913385826772,24.2913385826772,22.));
#3340=CARTESIAN_POINT('',(-0.354330708661419,25.,22.));
#3341=CARTESIAN_POINT('Origin',(0.,0.,0.708661417322834));
#3342=CARTESIAN_POINT('',(-35.2913385826772,25.,0.708661417322834));
#3343=CARTESIAN_POINT('',(-35.2913385826772,24.2913385826772,0.708661417322834));
#3344=CARTESIAN_POINT('',(-35.2913385826772,25.,0.708661417322834));
#3345=CARTESIAN_POINT('',(-0.354330708661419,25.,0.708661417322834));
#3346=CARTESIAN_POINT('',(-35.2913385826772,25.,0.708661417322834));
#3347=CARTESIAN_POINT('',(-0.354330708661419,24.2913385826772,0.708661417322834));
#3348=CARTESIAN_POINT('',(-0.354330708661419,25.,0.708661417322834));
#3349=CARTESIAN_POINT('',(-35.2913385826772,24.2913385826772,0.708661417322834));
#3350=CARTESIAN_POINT('Origin',(-35.2913385826772,25.,56.9441943703592));
#3351=CARTESIAN_POINT('',(-35.2913385826772,25.,22.));
#3352=CARTESIAN_POINT('',(-0.354330708661419,25.,22.));
#3353=CARTESIAN_POINT('Origin',(-0.354330708661419,25.,56.9441943703592));
#3354=CARTESIAN_POINT('',(-0.354330708661419,24.2913385826772,22.));
#3355=CARTESIAN_POINT('Origin',(-35.2913385826772,24.2913385826772,56.9441943703592));
#3356=CARTESIAN_POINT('',(-35.2913385826772,24.2913385826772,22.));
#3357=CARTESIAN_POINT('Origin',(-35.2913385826772,25.,56.9441943703592));
#3358=CARTESIAN_POINT('',(0.,0.,0.));
#3359=CARTESIAN_POINT('Origin',(22.9370078740157,0.,46.6558556092144));
#3360=CARTESIAN_POINT('',(22.9370078740157,4.64566929133858,22.));
#3361=CARTESIAN_POINT('',(22.9370078740157,4.64566929133858,0.708661417322834));
#3362=CARTESIAN_POINT('',(22.9370078740157,4.64566929133858,22.));
#3363=CARTESIAN_POINT('',(22.9370078740157,29.2913385826772,22.));
#3364=CARTESIAN_POINT('',(22.9370078740157,4.64566929133858,22.));
#3365=CARTESIAN_POINT('',(22.9370078740157,29.2913385826772,0.708661417322834));
#3366=CARTESIAN_POINT('',(22.9370078740157,29.2913385826772,22.));
#3367=CARTESIAN_POINT('',(22.9370078740157,4.64566929133858,0.708661417322834));
#3368=CARTESIAN_POINT('Origin',(0.,4.64566929133858,46.6558556092144));
#3369=CARTESIAN_POINT('',(23.6456692913386,4.64566929133858,22.));
#3370=CARTESIAN_POINT('',(23.6456692913386,4.64566929133858,0.708661417322834));
#3371=CARTESIAN_POINT('',(23.6456692913386,4.64566929133858,22.));
#3372=CARTESIAN_POINT('',(23.6456692913386,4.64566929133858,22.));
#3373=CARTESIAN_POINT('',(23.6456692913386,4.64566929133858,0.708661417322834));
#3374=CARTESIAN_POINT('Origin',(23.6456692913386,0.,46.6558556092144));
#3375=CARTESIAN_POINT('',(23.6456692913386,29.2913385826772,22.));
#3376=CARTESIAN_POINT('',(23.6456692913386,4.64566929133858,22.));
#3377=CARTESIAN_POINT('',(23.6456692913386,29.2913385826772,0.708661417322834));
#3378=CARTESIAN_POINT('',(23.6456692913386,4.64566929133858,0.708661417322834));
#3379=CARTESIAN_POINT('',(23.6456692913386,29.2913385826772,22.));
#3380=CARTESIAN_POINT('Origin',(0.,29.2913385826772,46.6558556092144));
#3381=CARTESIAN_POINT('',(23.6456692913386,29.2913385826772,22.));
#3382=CARTESIAN_POINT('',(23.6456692913386,29.2913385826772,0.708661417322834));
#3383=CARTESIAN_POINT('Origin',(0.,0.,0.708661417322834));
#3384=CARTESIAN_POINT('Origin',(0.,0.,22.));
#3385=CARTESIAN_POINT('',(0.,0.,0.));
#3386=CARTESIAN_POINT('Origin',(33.6377952755905,-4.91732638859567E-15,
19.6377952755906));
#3387=CARTESIAN_POINT('',(33.6377952755905,3.93700787401574,17.6692913385827));
#3388=CARTESIAN_POINT('Origin',(33.6377952755905,3.93700787401574,19.6377952755906));
#3389=CARTESIAN_POINT('',(33.6377952755905,-4.91732638859567E-15,17.6692913385827));
#3390=CARTESIAN_POINT('',(33.6377952755905,-4.91732638859567E-15,17.6692913385827));
#3391=CARTESIAN_POINT('Origin',(33.6377952755905,-4.91732638859567E-15,
19.6377952755906));
#3392=CARTESIAN_POINT('Origin',(33.6377952755905,-4.91732638859567E-15,
19.6377952755906));
#3393=CARTESIAN_POINT('Origin',(33.6377952755905,3.93700787401574,19.6377952755906));
#3394=CARTESIAN_POINT('',(0.,0.,0.));
#3395=CARTESIAN_POINT('Origin',(0.,0.,22.));
#3396=CARTESIAN_POINT('',(0.354330708661414,30.,22.));
#3397=CARTESIAN_POINT('',(35.2913385826772,30.,22.));
#3398=CARTESIAN_POINT('',(0.354330708661414,30.,22.));
#3399=CARTESIAN_POINT('',(0.354330708661414,29.2913385826772,22.));
#3400=CARTESIAN_POINT('',(0.354330708661414,30.,22.));
#3401=CARTESIAN_POINT('',(35.2913385826772,29.2913385826772,22.));
#3402=CARTESIAN_POINT('',(0.354330708661414,29.2913385826772,22.));
#3403=CARTESIAN_POINT('',(35.2913385826772,30.,22.));
#3404=CARTESIAN_POINT('Origin',(0.,0.,0.708661417322834));
#3405=CARTESIAN_POINT('',(0.354330708661414,30.,0.708661417322834));
#3406=CARTESIAN_POINT('',(0.354330708661414,29.2913385826772,0.708661417322834));
#3407=CARTESIAN_POINT('',(0.354330708661414,30.,0.708661417322834));
#3408=CARTESIAN_POINT('',(35.2913385826772,30.,0.708661417322834));
#3409=CARTESIAN_POINT('',(0.354330708661414,30.,0.708661417322834));
#3410=CARTESIAN_POINT('',(35.2913385826772,29.2913385826772,0.708661417322834));
#3411=CARTESIAN_POINT('',(35.2913385826772,30.,0.708661417322834));
#3412=CARTESIAN_POINT('',(0.354330708661414,29.2913385826772,0.708661417322834));
#3413=CARTESIAN_POINT('Origin',(0.354330708661414,30.,56.9441943703592));
#3414=CARTESIAN_POINT('',(0.354330708661414,30.,22.));
#3415=CARTESIAN_POINT('',(35.2913385826772,30.,22.));
#3416=CARTESIAN_POINT('Origin',(35.2913385826772,30.,56.9441943703592));
#3417=CARTESIAN_POINT('',(35.2913385826772,29.2913385826772,22.));
#3418=CARTESIAN_POINT('Origin',(0.354330708661414,29.2913385826772,56.9441943703592));
#3419=CARTESIAN_POINT('',(0.354330708661414,29.2913385826772,22.));
#3420=CARTESIAN_POINT('Origin',(0.354330708661414,30.,56.9441943703592));
#3421=CARTESIAN_POINT('',(0.,0.,0.));
#3422=CARTESIAN_POINT('Origin',(-35.2913385826772,-4.13304395193358E-15,
18.7086614173228));
#3423=CARTESIAN_POINT('',(-35.2913385826772,67.3543307086614,0.708661417322834));
#3424=CARTESIAN_POINT('',(-35.2913385826772,66.6456692913386,0.708661417322834));
#3425=CARTESIAN_POINT('',(-35.2913385826772,67.3543307086614,0.708661417322834));
#3426=CARTESIAN_POINT('',(-35.2913385826772,66.6456692913386,18.7086614173228));
#3427=CARTESIAN_POINT('',(-35.2913385826772,66.6456692913386,18.7086614173228));
#3428=CARTESIAN_POINT('',(-35.2913385826772,67.3543307086614,18.7086614173228));
#3429=CARTESIAN_POINT('',(-35.2913385826772,67.3543307086614,18.7086614173228));
#3430=CARTESIAN_POINT('',(-35.2913385826772,67.3543307086614,18.7086614173228));
#3431=CARTESIAN_POINT('Origin',(0.,66.6456692913386,18.7086614173228));
#3432=CARTESIAN_POINT('',(-0.354330708661425,66.6456692913386,0.708661417322834));
#3433=CARTESIAN_POINT('',(-35.2913385826772,66.6456692913386,0.708661417322834));
#3434=CARTESIAN_POINT('',(-0.354330708661425,66.6456692913386,18.7086614173228));
#3435=CARTESIAN_POINT('',(-0.354330708661425,66.6456692913386,18.7086614173228));
#3436=CARTESIAN_POINT('',(-35.2913385826772,66.6456692913386,18.7086614173228));
#3437=CARTESIAN_POINT('Origin',(-0.354330708661418,-3.50126087795579E-17,
18.7086614173228));
#3438=CARTESIAN_POINT('',(-0.354330708661425,67.3543307086614,0.708661417322834));
#3439=CARTESIAN_POINT('',(-0.354330708661425,66.6456692913386,0.708661417322834));
#3440=CARTESIAN_POINT('',(-0.354330708661425,67.3543307086614,18.7086614173228));
#3441=CARTESIAN_POINT('',(-0.354330708661425,67.3543307086614,18.7086614173228));
#3442=CARTESIAN_POINT('',(-0.354330708661425,66.6456692913386,18.7086614173228));
#3443=CARTESIAN_POINT('Origin',(0.,67.3543307086614,18.7086614173228));
#3444=CARTESIAN_POINT('',(-35.2913385826772,67.3543307086614,0.708661417322834));
#3445=CARTESIAN_POINT('',(-35.2913385826772,67.3543307086614,18.7086614173228));
#3446=CARTESIAN_POINT('Origin',(0.,0.,18.7086614173228));
#3447=CARTESIAN_POINT('Origin',(0.,0.,0.708661417322834));
#3448=CARTESIAN_POINT('',(0.,0.,0.));
#3449=CARTESIAN_POINT('Origin',(35.2913385826772,48.6771653543307,30.375872491424));
#3450=CARTESIAN_POINT('',(35.2913385826772,47.9685039370079,18.7086614173228));
#3451=CARTESIAN_POINT('',(35.2913385826772,48.6771653543307,18.7086614173228));
#3452=CARTESIAN_POINT('',(35.2913385826772,47.9685039370079,18.7086614173228));
#3453=CARTESIAN_POINT('',(35.2913385826772,47.9685039370079,0.708661417322834));
#3454=CARTESIAN_POINT('',(35.2913385826772,47.9685039370079,18.7086614173228));
#3455=CARTESIAN_POINT('',(35.2913385826772,48.6771653543307,0.708661417322834));
#3456=CARTESIAN_POINT('',(35.2913385826772,47.9685039370079,0.708661417322834));
#3457=CARTESIAN_POINT('',(35.2913385826772,48.6771653543307,18.7086614173228));
#3458=CARTESIAN_POINT('Origin',(23.6456692913386,48.6771653543307,30.375872491424));
#3459=CARTESIAN_POINT('',(23.6456692913386,48.6771653543307,18.7086614173228));
#3460=CARTESIAN_POINT('',(35.2913385826772,48.6771653543307,18.7086614173228));
#3461=CARTESIAN_POINT('',(23.6456692913386,48.6771653543307,0.708661417322834));
#3462=CARTESIAN_POINT('',(35.2913385826771,48.6771653543307,0.708661417322834));
#3463=CARTESIAN_POINT('',(23.6456692913386,48.6771653543307,18.7086614173228));
#3464=CARTESIAN_POINT('Origin',(23.6456692913386,48.6771653543307,30.375872491424));
#3465=CARTESIAN_POINT('',(23.6456692913386,47.9685039370079,18.7086614173228));
#3466=CARTESIAN_POINT('',(23.6456692913386,48.6771653543307,18.7086614173228));
#3467=CARTESIAN_POINT('',(23.6456692913386,47.9685039370079,0.708661417322834));
#3468=CARTESIAN_POINT('',(23.6456692913386,48.6771653543307,0.708661417322834));
#3469=CARTESIAN_POINT('',(23.6456692913386,47.9685039370079,18.7086614173228));
#3470=CARTESIAN_POINT('Origin',(23.6456692913386,47.9685039370079,30.375872491424));
#3471=CARTESIAN_POINT('',(23.6456692913386,47.9685039370079,18.7086614173228));
#3472=CARTESIAN_POINT('',(23.6456692913386,47.9685039370079,0.708661417322834));
#3473=CARTESIAN_POINT('Origin',(0.,0.,0.708661417322834));
#3474=CARTESIAN_POINT('Origin',(0.,0.,18.7086614173228));
#3475=CARTESIAN_POINT('',(0.,0.,0.));
#3476=CARTESIAN_POINT('Origin',(-12.7086614173228,66.6456692913386,60.3603597227694));
#3477=CARTESIAN_POINT('',(-12.7086614173228,66.6456692913386,18.7086614173228));
#3478=CARTESIAN_POINT('',(-12.7086614173228,25.,18.7086614173228));
#3479=CARTESIAN_POINT('',(-12.7086614173228,66.6456692913386,18.7086614173228));
#3480=CARTESIAN_POINT('',(-12.7086614173228,66.6456692913386,0.708661417322834));
#3481=CARTESIAN_POINT('',(-12.7086614173228,66.6456692913386,18.7086614173228));
#3482=CARTESIAN_POINT('',(-12.7086614173228,25.,0.708661417322834));
#3483=CARTESIAN_POINT('',(-12.7086614173228,66.6456692913386,0.708661417322834));
#3484=CARTESIAN_POINT('',(-12.7086614173228,25.,18.7086614173228));
#3485=CARTESIAN_POINT('Origin',(-12.7086614173228,25.,60.3603597227694));
#3486=CARTESIAN_POINT('',(-12.,25.,18.7086614173228));
#3487=CARTESIAN_POINT('',(-12.7086614173228,25.,18.7086614173228));
#3488=CARTESIAN_POINT('',(-12.,25.,0.708661417322834));
#3489=CARTESIAN_POINT('',(-12.7086614173228,25.,0.708661417322834));
#3490=CARTESIAN_POINT('',(-12.,25.,18.7086614173228));
#3491=CARTESIAN_POINT('Origin',(-12.,66.6456692913386,60.3603597227694));
#3492=CARTESIAN_POINT('',(-12.,66.6456692913386,18.7086614173228));
#3493=CARTESIAN_POINT('',(-12.,25.,18.7086614173228));
#3494=CARTESIAN_POINT('',(-12.,66.6456692913386,0.708661417322834));
#3495=CARTESIAN_POINT('',(-12.,25.,0.708661417322834));
#3496=CARTESIAN_POINT('',(-12.,66.6456692913386,18.7086614173228));
#3497=CARTESIAN_POINT('Origin',(-12.7086614173228,66.6456692913386,60.3603597227694));
#3498=CARTESIAN_POINT('',(-12.,66.6456692913386,18.7086614173228));
#3499=CARTESIAN_POINT('',(-12.,66.6456692913386,0.708661417322834));
#3500=CARTESIAN_POINT('Origin',(0.,0.,0.708661417322834));
#3501=CARTESIAN_POINT('Origin',(0.,0.,18.7086614173228));
#3502=CARTESIAN_POINT('',(0.,0.,0.));
#3503=CARTESIAN_POINT('Origin',(-36.,80.0000000000007,1.44950256676235E-46));
#3504=CARTESIAN_POINT('',(-36.,79.2913385826778,1.36251621821105E-58));
#3505=CARTESIAN_POINT('',(-36.,79.2913385826778,22.));
#3506=CARTESIAN_POINT('',(-36.,79.2913385826778,1.36251621821105E-58));
#3507=CARTESIAN_POINT('',(-36.,80.0000000000007,22.));
#3508=CARTESIAN_POINT('',(-36.,80.0000000000007,22.));
#3509=CARTESIAN_POINT('',(-36.,80.0000000000007,1.44950256676235E-46));
#3510=CARTESIAN_POINT('',(-36.,80.0000000000007,1.44950256676235E-46));
#3511=CARTESIAN_POINT('',(-36.,80.0000000000007,1.44950256676235E-46));
#3512=CARTESIAN_POINT('Origin',(-36.,80.0000000000007,22.));
#3513=CARTESIAN_POINT('',(36.,79.2913385826765,22.));
#3514=CARTESIAN_POINT('',(-36.,79.2913385826778,22.));
#3515=CARTESIAN_POINT('',(36.,79.9999999999993,22.));
#3516=CARTESIAN_POINT('',(36.,79.9999999999993,22.));
#3517=CARTESIAN_POINT('',(-36.,80.0000000000007,22.));
#3518=CARTESIAN_POINT('Origin',(36.,79.9999999999993,1.44950256675963E-46));
#3519=CARTESIAN_POINT('',(36.,79.2913385826765,-1.36251621821105E-58));
#3520=CARTESIAN_POINT('',(36.,79.2913385826765,22.));
#3521=CARTESIAN_POINT('',(36.,79.9999999999993,1.44950256675963E-46));
#3522=CARTESIAN_POINT('',(36.,79.9999999999993,1.44950256675963E-46));
#3523=CARTESIAN_POINT('',(36.,79.9999999999993,22.));
#3524=CARTESIAN_POINT('Origin',(-36.,80.0000000000007,1.44950256676235E-46));
#3525=CARTESIAN_POINT('',(36.,79.2913385826765,-1.36251621821105E-58));
#3526=CARTESIAN_POINT('',(36.,79.9999999999993,1.44950256675963E-46));
#3527=CARTESIAN_POINT('Origin',(1.47644648822515E-12,80.,-2.90734909672741E-28));
#3528=CARTESIAN_POINT('Origin',(1.46333361785556E-12,79.2913385826772,-2.90734909672741E-28));
#3529=CARTESIAN_POINT('',(0.,0.,0.));
#3530=CARTESIAN_POINT('Origin',(-33.6377952755905,-4.91732638859567E-15,
19.6377952755906));
#3531=CARTESIAN_POINT('',(-33.6377952755905,3.93700787401574,17.6692913385827));
#3532=CARTESIAN_POINT('Origin',(-33.6377952755905,3.93700787401574,19.6377952755906));
#3533=CARTESIAN_POINT('',(-33.6377952755905,-4.91732638859567E-15,17.6692913385827));
#3534=CARTESIAN_POINT('',(-33.6377952755905,-4.91732638859567E-15,17.6692913385827));
#3535=CARTESIAN_POINT('Origin',(-33.6377952755905,-4.91732638859567E-15,
19.6377952755906));
#3536=CARTESIAN_POINT('Origin',(-33.6377952755905,-4.91732638859567E-15,
19.6377952755906));
#3537=CARTESIAN_POINT('Origin',(-33.6377952755905,3.93700787401574,19.6377952755906));
#3538=CARTESIAN_POINT('',(0.,0.,0.));
#3539=CARTESIAN_POINT('Origin',(33.6377952755906,-4.91732638859567E-15,
2.36220472440945));
#3540=CARTESIAN_POINT('',(33.6377952755906,3.93700787401574,0.393700787401574));
#3541=CARTESIAN_POINT('Origin',(33.6377952755906,3.93700787401574,2.36220472440945));
#3542=CARTESIAN_POINT('',(33.6377952755906,-4.91732638859567E-15,0.393700787401574));
#3543=CARTESIAN_POINT('',(33.6377952755906,-4.91732638859567E-15,0.393700787401574));
#3544=CARTESIAN_POINT('Origin',(33.6377952755906,-4.91732638859567E-15,
2.36220472440945));
#3545=CARTESIAN_POINT('Origin',(33.6377952755906,-4.91732638859567E-15,
2.36220472440945));
#3546=CARTESIAN_POINT('Origin',(33.6377952755906,3.93700787401574,2.36220472440945));
#3547=CARTESIAN_POINT('',(0.,0.,0.));
#3548=CARTESIAN_POINT('Origin',(-33.6377952755905,-4.91732638859567E-15,
2.36220472440945));
#3549=CARTESIAN_POINT('',(-33.6377952755905,3.93700787401574,0.393700787401579));
#3550=CARTESIAN_POINT('Origin',(-33.6377952755905,3.93700787401574,2.36220472440945));
#3551=CARTESIAN_POINT('',(-33.6377952755905,-4.91732638859567E-15,0.393700787401579));
#3552=CARTESIAN_POINT('',(-33.6377952755905,-4.91732638859567E-15,0.393700787401579));
#3553=CARTESIAN_POINT('Origin',(-33.6377952755905,-4.91732638859567E-15,
2.36220472440945));
#3554=CARTESIAN_POINT('Origin',(-33.6377952755905,-4.91732638859567E-15,
2.36220472440945));
#3555=CARTESIAN_POINT('Origin',(-33.6377952755905,3.93700787401574,2.36220472440945));
#3556=CARTESIAN_POINT('',(0.,0.,0.));
#3557=CARTESIAN_POINT('Origin',(1.31128703695885E-14,-4.91732638859567E-15,
2.36220472440945));
#3558=CARTESIAN_POINT('',(1.31128703695885E-14,3.93700787401574,0.393700787401575));
#3559=CARTESIAN_POINT('Origin',(1.31128703695885E-14,3.93700787401574,2.36220472440945));
#3560=CARTESIAN_POINT('',(1.31128703695885E-14,-4.91732638859567E-15,0.393700787401575));
#3561=CARTESIAN_POINT('',(1.28717981650319E-14,-4.91732638859567E-15,0.393700787401575));
#3562=CARTESIAN_POINT('Origin',(1.31128703695885E-14,-4.91732638859567E-15,
2.36220472440945));
#3563=CARTESIAN_POINT('Origin',(1.31128703695885E-14,-4.91732638859567E-15,
2.36220472440945));
#3564=CARTESIAN_POINT('Origin',(1.31128703695885E-14,3.93700787401574,2.36220472440945));
#3565=CARTESIAN_POINT('',(0.,0.,0.));
#3566=CARTESIAN_POINT('Origin',(-35.2913385826772,79.2913385826772,0.708661417322834));
#3567=CARTESIAN_POINT('',(-35.2913385826772,79.2913385826772,0.));
#3568=CARTESIAN_POINT('',(-35.2913385826772,4.64566929133858,0.));
#3569=CARTESIAN_POINT('',(-35.2913385826772,79.2913385826772,0.));
#3570=CARTESIAN_POINT('',(-35.2913385826772,4.64566929133858,0.708661417322834));
#3571=CARTESIAN_POINT('',(-35.2913385826772,4.64566929133858,0.708661417322834));
#3572=CARTESIAN_POINT('',(-35.2913385826772,79.2913385826772,0.708661417322834));
#3573=CARTESIAN_POINT('',(-35.2913385826772,79.2913385826772,0.708661417322834));
#3574=CARTESIAN_POINT('',(-35.2913385826772,79.2913385826772,0.708661417322834));
#3575=CARTESIAN_POINT('Origin',(-35.2913385826772,4.64566929133858,0.708661417322834));
#3576=CARTESIAN_POINT('',(-0.354330708661419,4.64566929133858,0.));
#3577=CARTESIAN_POINT('',(-35.2913385826772,4.64566929133858,0.));
#3578=CARTESIAN_POINT('',(-0.354330708661419,4.64566929133858,0.708661417322834));
#3579=CARTESIAN_POINT('',(-0.354330708661419,4.64566929133858,0.708661417322834));
#3580=CARTESIAN_POINT('',(-35.2913385826772,4.64566929133858,0.708661417322834));
#3581=CARTESIAN_POINT('Origin',(-0.354330708661426,79.2913385826772,0.708661417322834));
#3582=CARTESIAN_POINT('',(-0.354330708661426,79.2913385826772,0.));
#3583=CARTESIAN_POINT('',(-0.354330708661419,4.64566929133858,0.));
#3584=CARTESIAN_POINT('',(-0.354330708661426,79.2913385826772,0.708661417322834));
#3585=CARTESIAN_POINT('',(-0.354330708661426,79.2913385826772,0.708661417322834));
#3586=CARTESIAN_POINT('',(-0.354330708661419,4.64566929133858,0.708661417322834));
#3587=CARTESIAN_POINT('Origin',(-35.2913385826772,79.2913385826772,0.708661417322834));
#3588=CARTESIAN_POINT('',(-0.354330708661426,79.2913385826772,0.));
#3589=CARTESIAN_POINT('',(-0.354330708661426,79.2913385826772,0.708661417322834));
#3590=CARTESIAN_POINT('Origin',(0.,0.,0.708661417322834));
#3591=CARTESIAN_POINT('Origin',(0.,0.,0.));
#3592=CARTESIAN_POINT('',(0.,0.,0.));
#3593=CARTESIAN_POINT('Origin',(-36.,3.93700787401574,22.));
#3594=CARTESIAN_POINT('',(-36.,4.64566929133858,22.));
#3595=CARTESIAN_POINT('',(-36.,4.64566929133858,0.));
#3596=CARTESIAN_POINT('',(-36.,4.64566929133858,22.));
#3597=CARTESIAN_POINT('',(-36.,3.93700787401574,0.));
#3598=CARTESIAN_POINT('',(-36.,3.93700787401574,0.));
#3599=CARTESIAN_POINT('',(-36.,3.93700787401574,22.));
#3600=CARTESIAN_POINT('',(-36.,3.93700787401574,22.));
#3601=CARTESIAN_POINT('',(-36.,3.93700787401574,22.));
#3602=CARTESIAN_POINT('Origin',(-36.,3.93700787401574,0.));
#3603=CARTESIAN_POINT('',(36.,4.64566929133858,0.));
#3604=CARTESIAN_POINT('',(-36.,4.64566929133858,0.));
#3605=CARTESIAN_POINT('',(36.,3.93700787401574,0.));
#3606=CARTESIAN_POINT('',(36.,3.93700787401574,0.));
#3607=CARTESIAN_POINT('',(-36.,3.93700787401574,0.));
#3608=CARTESIAN_POINT('Origin',(36.,3.93700787401574,22.));
#3609=CARTESIAN_POINT('',(36.,4.64566929133858,22.));
#3610=CARTESIAN_POINT('',(36.,4.64566929133858,0.));
#3611=CARTESIAN_POINT('',(36.,3.93700787401574,22.));
#3612=CARTESIAN_POINT('',(36.,3.93700787401574,22.));
#3613=CARTESIAN_POINT('',(36.,3.93700787401574,0.));
#3614=CARTESIAN_POINT('Origin',(-36.,3.93700787401574,22.));
#3615=CARTESIAN_POINT('',(36.,4.64566929133858,22.));
#3616=CARTESIAN_POINT('',(36.,3.93700787401574,22.));
#3617=CARTESIAN_POINT('Origin',(0.,3.93700787401574,0.));
#3618=CARTESIAN_POINT('Origin',(0.,4.64566929133858,0.));
#3619=CARTESIAN_POINT('',(0.,0.,0.));
#3620=CARTESIAN_POINT('Origin',(0.354330708661416,4.64566929133858,0.708661417322834));
#3621=CARTESIAN_POINT('',(0.354330708661416,79.2913385826772,0.));
#3622=CARTESIAN_POINT('',(0.354330708661416,4.64566929133858,0.));
#3623=CARTESIAN_POINT('',(0.354330708661416,79.2913385826772,0.));
#3624=CARTESIAN_POINT('',(0.354330708661416,4.64566929133858,0.708661417322834));
#3625=CARTESIAN_POINT('',(0.354330708661416,4.64566929133858,0.708661417322834));
#3626=CARTESIAN_POINT('',(0.354330708661416,79.2913385826772,0.708661417322834));
#3627=CARTESIAN_POINT('',(0.354330708661416,79.2913385826772,0.708661417322834));
#3628=CARTESIAN_POINT('',(0.354330708661416,79.2913385826772,0.708661417322834));
#3629=CARTESIAN_POINT('Origin',(0.354330708661416,4.64566929133858,0.708661417322834));
#3630=CARTESIAN_POINT('',(35.2913385826772,4.64566929133858,0.));
#3631=CARTESIAN_POINT('',(0.354330708661416,4.64566929133858,0.));
#3632=CARTESIAN_POINT('',(35.2913385826772,4.64566929133858,0.708661417322834));
#3633=CARTESIAN_POINT('',(35.2913385826772,4.64566929133858,0.708661417322834));
#3634=CARTESIAN_POINT('',(0.354330708661416,4.64566929133858,0.708661417322834));
#3635=CARTESIAN_POINT('Origin',(35.2913385826772,4.64566929133858,0.708661417322834));
#3636=CARTESIAN_POINT('',(35.2913385826772,79.2913385826772,0.));
#3637=CARTESIAN_POINT('',(35.2913385826772,4.64566929133858,0.));
#3638=CARTESIAN_POINT('',(35.2913385826772,79.2913385826772,0.708661417322834));
#3639=CARTESIAN_POINT('',(35.2913385826772,79.2913385826772,0.708661417322834));
#3640=CARTESIAN_POINT('',(35.2913385826772,4.64566929133858,0.708661417322834));
#3641=CARTESIAN_POINT('Origin',(0.354330708661416,79.2913385826772,0.708661417322834));
#3642=CARTESIAN_POINT('',(35.2913385826772,79.2913385826772,0.));
#3643=CARTESIAN_POINT('',(35.2913385826772,79.2913385826772,0.708661417322834));
#3644=CARTESIAN_POINT('Origin',(0.,0.,0.708661417322834));
#3645=CARTESIAN_POINT('Origin',(0.,0.,0.));
#3646=CARTESIAN_POINT('',(51.2961940801881,26.9850681841422,67.8171719943154));
#3647=CARTESIAN_POINT('',(51.2961940801881,26.9850681841422,67.8171719943154));
#3648=CARTESIAN_POINT('',(51.2961940801881,26.9850681841422,67.8171719943154));
#3649=CARTESIAN_POINT('',(51.2961940801881,26.9850681841422,67.8171719943154));
#3650=CARTESIAN_POINT('',(51.2961940801881,26.9850681841422,67.8171719943154));
#3651=CARTESIAN_POINT('',(51.2961940801881,26.9850681841422,67.8171719943154));
#3652=CARTESIAN_POINT('',(51.2961940801881,26.9850681841422,67.8171719943154));
#3653=CARTESIAN_POINT('',(51.2961940801881,26.9850681841422,67.8171719943154));
#3654=CARTESIAN_POINT('',(51.2961940801881,26.9850681841422,67.8171719943154));
#3655=CARTESIAN_POINT('',(51.2961940801881,26.9850681841422,67.8171719943154));
#3656=CARTESIAN_POINT('',(51.2961940801881,26.9850681841422,67.8171719943154));
#3657=CARTESIAN_POINT('',(51.2961940801881,26.9850681841422,67.8171719943154));
#3658=CARTESIAN_POINT('',(51.2961940801881,26.9850681841422,67.8171719943154));
#3659=CARTESIAN_POINT('',(51.2961940801881,26.9850681841422,67.8171719943154));
#3660=CARTESIAN_POINT('',(51.2961940801881,26.9850681841422,67.8171719943154));
#3661=CARTESIAN_POINT('',(51.2961940801881,26.9850681841422,67.8171719943154));
#3662=CARTESIAN_POINT('',(51.2961940801881,26.9850681841422,67.8171719943154));
#3663=CARTESIAN_POINT('',(51.2961940801881,26.9850681841422,67.8171719943154));
#3664=CARTESIAN_POINT('',(51.2961940801881,26.9850681841422,67.8171719943154));
#3665=CARTESIAN_POINT('',(51.2961940801881,26.9850681841422,67.8171719943154));
#3666=CARTESIAN_POINT('',(51.2961940801881,26.9850681841422,67.8171719943154));
#3667=CARTESIAN_POINT('',(51.2961940801881,26.9850681841422,67.8171719943154));
#3668=CARTESIAN_POINT('',(51.2961940801881,26.9850681841422,67.8171719943154));
#3669=CARTESIAN_POINT('',(51.2961940801881,26.9850681841422,67.8171719943154));
#3670=UNCERTAINTY_MEASURE_WITH_UNIT(LENGTH_MEASURE(0.000393700787401575),
#3725,'DISTANCE_ACCURACY_VALUE',
'Maximum model space distance between geometric entities at asserted c
onnectivities');
#3671=UNCERTAINTY_MEASURE_WITH_UNIT(LENGTH_MEASURE(0.000393700787401575),
#3725,'DISTANCE_ACCURACY_VALUE',
'Maximum model space distance between geometric entities at asserted c
onnectivities');
#3672=UNCERTAINTY_MEASURE_WITH_UNIT(LENGTH_MEASURE(0.000393700787401575),
#3725,'DISTANCE_ACCURACY_VALUE',
'Maximum model space distance between geometric entities at asserted c
onnectivities');
#3673=UNCERTAINTY_MEASURE_WITH_UNIT(LENGTH_MEASURE(0.000393700787401575),
#3725,'DISTANCE_ACCURACY_VALUE',
'Maximum model space distance between geometric entities at asserted c
onnectivities');
#3674=UNCERTAINTY_MEASURE_WITH_UNIT(LENGTH_MEASURE(0.000393700787401575),
#3725,'DISTANCE_ACCURACY_VALUE',
'Maximum model space distance between geometric entities at asserted c
onnectivities');
#3675=UNCERTAINTY_MEASURE_WITH_UNIT(LENGTH_MEASURE(0.000393700787401575),
#3725,'DISTANCE_ACCURACY_VALUE',
'Maximum model space distance between geometric entities at asserted c
onnectivities');
#3676=UNCERTAINTY_MEASURE_WITH_UNIT(LENGTH_MEASURE(0.000393700787401575),
#3725,'DISTANCE_ACCURACY_VALUE',
'Maximum model space distance between geometric entities at asserted c
onnectivities');
#3677=UNCERTAINTY_MEASURE_WITH_UNIT(LENGTH_MEASURE(0.000393700787401575),
#3725,'DISTANCE_ACCURACY_VALUE',
'Maximum model space distance between geometric entities at asserted c
onnectivities');
#3678=UNCERTAINTY_MEASURE_WITH_UNIT(LENGTH_MEASURE(0.000393700787401575),
#3725,'DISTANCE_ACCURACY_VALUE',
'Maximum model space distance between geometric entities at asserted c
onnectivities');
#3679=UNCERTAINTY_MEASURE_WITH_UNIT(LENGTH_MEASURE(0.000393700787401575),
#3725,'DISTANCE_ACCURACY_VALUE',
'Maximum model space distance between geometric entities at asserted c
onnectivities');
#3680=UNCERTAINTY_MEASURE_WITH_UNIT(LENGTH_MEASURE(0.000393700787401575),
#3725,'DISTANCE_ACCURACY_VALUE',
'Maximum model space distance between geometric entities at asserted c
onnectivities');
#3681=UNCERTAINTY_MEASURE_WITH_UNIT(LENGTH_MEASURE(0.000393700787401575),
#3725,'DISTANCE_ACCURACY_VALUE',
'Maximum model space distance between geometric entities at asserted c
onnectivities');
#3682=UNCERTAINTY_MEASURE_WITH_UNIT(LENGTH_MEASURE(0.000393700787401575),
#3725,'DISTANCE_ACCURACY_VALUE',
'Maximum model space distance between geometric entities at asserted c
onnectivities');
#3683=UNCERTAINTY_MEASURE_WITH_UNIT(LENGTH_MEASURE(0.000393700787401575),
#3725,'DISTANCE_ACCURACY_VALUE',
'Maximum model space distance between geometric entities at asserted c
onnectivities');
#3684=UNCERTAINTY_MEASURE_WITH_UNIT(LENGTH_MEASURE(0.000393700787401575),
#3725,'DISTANCE_ACCURACY_VALUE',
'Maximum model space distance between geometric entities at asserted c
onnectivities');
#3685=UNCERTAINTY_MEASURE_WITH_UNIT(LENGTH_MEASURE(0.000393700787401575),
#3725,'DISTANCE_ACCURACY_VALUE',
'Maximum model space distance between geometric entities at asserted c
onnectivities');
#3686=UNCERTAINTY_MEASURE_WITH_UNIT(LENGTH_MEASURE(0.000393700787401575),
#3725,'DISTANCE_ACCURACY_VALUE',
'Maximum model space distance between geometric entities at asserted c
onnectivities');
#3687=UNCERTAINTY_MEASURE_WITH_UNIT(LENGTH_MEASURE(0.000393700787401575),
#3725,'DISTANCE_ACCURACY_VALUE',
'Maximum model space distance between geometric entities at asserted c
onnectivities');
#3688=UNCERTAINTY_MEASURE_WITH_UNIT(LENGTH_MEASURE(0.000393700787401575),
#3725,'DISTANCE_ACCURACY_VALUE',
'Maximum model space distance between geometric entities at asserted c
onnectivities');
#3689=UNCERTAINTY_MEASURE_WITH_UNIT(LENGTH_MEASURE(0.000393700787401575),
#3725,'DISTANCE_ACCURACY_VALUE',
'Maximum model space distance between geometric entities at asserted c
onnectivities');
#3690=UNCERTAINTY_MEASURE_WITH_UNIT(LENGTH_MEASURE(0.000393700787401575),
#3725,'DISTANCE_ACCURACY_VALUE',
'Maximum model space distance between geometric entities at asserted c
onnectivities');
#3691=UNCERTAINTY_MEASURE_WITH_UNIT(LENGTH_MEASURE(0.000393700787401575),
#3725,'DISTANCE_ACCURACY_VALUE',
'Maximum model space distance between geometric entities at asserted c
onnectivities');
#3692=UNCERTAINTY_MEASURE_WITH_UNIT(LENGTH_MEASURE(0.000393700787401575),
#3725,'DISTANCE_ACCURACY_VALUE',
'Maximum model space distance between geometric entities at asserted c
onnectivities');
#3693=UNCERTAINTY_MEASURE_WITH_UNIT(LENGTH_MEASURE(0.000393700787401575),
#3725,'DISTANCE_ACCURACY_VALUE',
'Maximum model space distance between geometric entities at asserted c
onnectivities');
#3694=UNCERTAINTY_MEASURE_WITH_UNIT(LENGTH_MEASURE(0.000393700787401575),
#3725,'DISTANCE_ACCURACY_VALUE',
'Maximum model space distance between geometric entities at asserted c
onnectivities');
#3695=UNCERTAINTY_MEASURE_WITH_UNIT(LENGTH_MEASURE(0.000393700787401575),
#3725,'DISTANCE_ACCURACY_VALUE',
'Maximum model space distance between geometric entities at asserted c
onnectivities');
#3696=UNCERTAINTY_MEASURE_WITH_UNIT(LENGTH_MEASURE(0.000393700787401575),
#3725,'DISTANCE_ACCURACY_VALUE',
'Maximum model space distance between geometric entities at asserted c
onnectivities');
#3697=(
GEOMETRIC_REPRESENTATION_CONTEXT(3)
GLOBAL_UNCERTAINTY_ASSIGNED_CONTEXT((#3670))
GLOBAL_UNIT_ASSIGNED_CONTEXT((#3725,#3729,#3730))
REPRESENTATION_CONTEXT('','3D')
);
#3698=(
GEOMETRIC_REPRESENTATION_CONTEXT(3)
GLOBAL_UNCERTAINTY_ASSIGNED_CONTEXT((#3671))
GLOBAL_UNIT_ASSIGNED_CONTEXT((#3725,#3729,#3730))
REPRESENTATION_CONTEXT('','3D')
);
#3699=(
GEOMETRIC_REPRESENTATION_CONTEXT(3)
GLOBAL_UNCERTAINTY_ASSIGNED_CONTEXT((#3672))
GLOBAL_UNIT_ASSIGNED_CONTEXT((#3725,#3729,#3730))
REPRESENTATION_CONTEXT('','3D')
);
#3700=(
GEOMETRIC_REPRESENTATION_CONTEXT(3)
GLOBAL_UNCERTAINTY_ASSIGNED_CONTEXT((#3673))
GLOBAL_UNIT_ASSIGNED_CONTEXT((#3725,#3729,#3730))
REPRESENTATION_CONTEXT('','3D')
);
#3701=(
GEOMETRIC_REPRESENTATION_CONTEXT(3)
GLOBAL_UNCERTAINTY_ASSIGNED_CONTEXT((#3674))
GLOBAL_UNIT_ASSIGNED_CONTEXT((#3725,#3729,#3730))
REPRESENTATION_CONTEXT('','3D')
);
#3702=(
GEOMETRIC_REPRESENTATION_CONTEXT(3)
GLOBAL_UNCERTAINTY_ASSIGNED_CONTEXT((#3675))
GLOBAL_UNIT_ASSIGNED_CONTEXT((#3725,#3729,#3730))
REPRESENTATION_CONTEXT('','3D')
);
#3703=(
GEOMETRIC_REPRESENTATION_CONTEXT(3)
GLOBAL_UNCERTAINTY_ASSIGNED_CONTEXT((#3676))
GLOBAL_UNIT_ASSIGNED_CONTEXT((#3725,#3729,#3730))
REPRESENTATION_CONTEXT('','3D')
);
#3704=(
GEOMETRIC_REPRESENTATION_CONTEXT(3)
GLOBAL_UNCERTAINTY_ASSIGNED_CONTEXT((#3677))
GLOBAL_UNIT_ASSIGNED_CONTEXT((#3725,#3729,#3730))
REPRESENTATION_CONTEXT('','3D')
);
#3705=(
GEOMETRIC_REPRESENTATION_CONTEXT(3)
GLOBAL_UNCERTAINTY_ASSIGNED_CONTEXT((#3678))
GLOBAL_UNIT_ASSIGNED_CONTEXT((#3725,#3729,#3730))
REPRESENTATION_CONTEXT('','3D')
);
#3706=(
GEOMETRIC_REPRESENTATION_CONTEXT(3)
GLOBAL_UNCERTAINTY_ASSIGNED_CONTEXT((#3679))
GLOBAL_UNIT_ASSIGNED_CONTEXT((#3725,#3729,#3730))
REPRESENTATION_CONTEXT('','3D')
);
#3707=(
GEOMETRIC_REPRESENTATION_CONTEXT(3)
GLOBAL_UNCERTAINTY_ASSIGNED_CONTEXT((#3680))
GLOBAL_UNIT_ASSIGNED_CONTEXT((#3725,#3729,#3730))
REPRESENTATION_CONTEXT('','3D')
);
#3708=(
GEOMETRIC_REPRESENTATION_CONTEXT(3)
GLOBAL_UNCERTAINTY_ASSIGNED_CONTEXT((#3681))
GLOBAL_UNIT_ASSIGNED_CONTEXT((#3725,#3729,#3730))
REPRESENTATION_CONTEXT('','3D')
);
#3709=(
GEOMETRIC_REPRESENTATION_CONTEXT(3)
GLOBAL_UNCERTAINTY_ASSIGNED_CONTEXT((#3682))
GLOBAL_UNIT_ASSIGNED_CONTEXT((#3725,#3729,#3730))
REPRESENTATION_CONTEXT('','3D')
);
#3710=(
GEOMETRIC_REPRESENTATION_CONTEXT(3)
GLOBAL_UNCERTAINTY_ASSIGNED_CONTEXT((#3683))
GLOBAL_UNIT_ASSIGNED_CONTEXT((#3725,#3729,#3730))
REPRESENTATION_CONTEXT('','3D')
);
#3711=(
GEOMETRIC_REPRESENTATION_CONTEXT(3)
GLOBAL_UNCERTAINTY_ASSIGNED_CONTEXT((#3684))
GLOBAL_UNIT_ASSIGNED_CONTEXT((#3725,#3729,#3730))
REPRESENTATION_CONTEXT('','3D')
);
#3712=(
GEOMETRIC_REPRESENTATION_CONTEXT(3)
GLOBAL_UNCERTAINTY_ASSIGNED_CONTEXT((#3685))
GLOBAL_UNIT_ASSIGNED_CONTEXT((#3725,#3729,#3730))
REPRESENTATION_CONTEXT('','3D')
);
#3713=(
GEOMETRIC_REPRESENTATION_CONTEXT(3)
GLOBAL_UNCERTAINTY_ASSIGNED_CONTEXT((#3686))
GLOBAL_UNIT_ASSIGNED_CONTEXT((#3725,#3729,#3730))
REPRESENTATION_CONTEXT('','3D')
);
#3714=(
GEOMETRIC_REPRESENTATION_CONTEXT(3)
GLOBAL_UNCERTAINTY_ASSIGNED_CONTEXT((#3687))
GLOBAL_UNIT_ASSIGNED_CONTEXT((#3725,#3729,#3730))
REPRESENTATION_CONTEXT('','3D')
);
#3715=(
GEOMETRIC_REPRESENTATION_CONTEXT(3)
GLOBAL_UNCERTAINTY_ASSIGNED_CONTEXT((#3688))
GLOBAL_UNIT_ASSIGNED_CONTEXT((#3725,#3729,#3730))
REPRESENTATION_CONTEXT('','3D')
);
#3716=(
GEOMETRIC_REPRESENTATION_CONTEXT(3)
GLOBAL_UNCERTAINTY_ASSIGNED_CONTEXT((#3689))
GLOBAL_UNIT_ASSIGNED_CONTEXT((#3725,#3729,#3730))
REPRESENTATION_CONTEXT('','3D')
);
#3717=(
GEOMETRIC_REPRESENTATION_CONTEXT(3)
GLOBAL_UNCERTAINTY_ASSIGNED_CONTEXT((#3690))
GLOBAL_UNIT_ASSIGNED_CONTEXT((#3725,#3729,#3730))
REPRESENTATION_CONTEXT('','3D')
);
#3718=(
GEOMETRIC_REPRESENTATION_CONTEXT(3)
GLOBAL_UNCERTAINTY_ASSIGNED_CONTEXT((#3691))
GLOBAL_UNIT_ASSIGNED_CONTEXT((#3725,#3729,#3730))
REPRESENTATION_CONTEXT('','3D')
);
#3719=(
GEOMETRIC_REPRESENTATION_CONTEXT(3)
GLOBAL_UNCERTAINTY_ASSIGNED_CONTEXT((#3692))
GLOBAL_UNIT_ASSIGNED_CONTEXT((#3725,#3729,#3730))
REPRESENTATION_CONTEXT('','3D')
);
#3720=(
GEOMETRIC_REPRESENTATION_CONTEXT(3)
GLOBAL_UNCERTAINTY_ASSIGNED_CONTEXT((#3693))
GLOBAL_UNIT_ASSIGNED_CONTEXT((#3725,#3729,#3730))
REPRESENTATION_CONTEXT('','3D')
);
#3721=(
GEOMETRIC_REPRESENTATION_CONTEXT(3)
GLOBAL_UNCERTAINTY_ASSIGNED_CONTEXT((#3694))
GLOBAL_UNIT_ASSIGNED_CONTEXT((#3725,#3729,#3730))
REPRESENTATION_CONTEXT('','3D')
);
#3722=(
GEOMETRIC_REPRESENTATION_CONTEXT(3)
GLOBAL_UNCERTAINTY_ASSIGNED_CONTEXT((#3695))
GLOBAL_UNIT_ASSIGNED_CONTEXT((#3725,#3729,#3730))
REPRESENTATION_CONTEXT('','3D')
);
#3723=(
GEOMETRIC_REPRESENTATION_CONTEXT(3)
GLOBAL_UNCERTAINTY_ASSIGNED_CONTEXT((#3696))
GLOBAL_UNIT_ASSIGNED_CONTEXT((#3725,#3729,#3730))
REPRESENTATION_CONTEXT('','3D')
);
#3724=DIMENSIONAL_EXPONENTS(1.,0.,0.,0.,0.,0.,0.);
#3725=(
CONVERSION_BASED_UNIT('inch',#3728)
LENGTH_UNIT()
NAMED_UNIT(#3724)
);
#3726=(
LENGTH_UNIT()
NAMED_UNIT(*)
SI_UNIT(.MILLI.,.METRE.)
);
#3727=(
LENGTH_UNIT()
NAMED_UNIT(*)
SI_UNIT($,.METRE.)
);
#3728=LENGTH_MEASURE_WITH_UNIT(LENGTH_MEASURE(25.4),#3726);
#3729=(
NAMED_UNIT(*)
PLANE_ANGLE_UNIT()
SI_UNIT($,.RADIAN.)
);
#3730=(
NAMED_UNIT(*)
SI_UNIT($,.STERADIAN.)
SOLID_ANGLE_UNIT()
);
#3731=SHAPE_DEFINITION_REPRESENTATION(#3757,#3808);
#3732=SHAPE_DEFINITION_REPRESENTATION(#3758,#3809);
#3733=SHAPE_DEFINITION_REPRESENTATION(#3759,#3810);
#3734=SHAPE_DEFINITION_REPRESENTATION(#3761,#3811);
#3735=SHAPE_DEFINITION_REPRESENTATION(#3762,#3812);
#3736=SHAPE_DEFINITION_REPRESENTATION(#3763,#3813);
#3737=SHAPE_DEFINITION_REPRESENTATION(#3764,#3814);
#3738=SHAPE_DEFINITION_REPRESENTATION(#3765,#3815);
#3739=SHAPE_DEFINITION_REPRESENTATION(#3766,#3816);
#3740=SHAPE_DEFINITION_REPRESENTATION(#3767,#3817);
#3741=SHAPE_DEFINITION_REPRESENTATION(#3768,#3818);
#3742=SHAPE_DEFINITION_REPRESENTATION(#3769,#3819);
#3743=SHAPE_DEFINITION_REPRESENTATION(#3770,#3820);
#3744=SHAPE_DEFINITION_REPRESENTATION(#3771,#3821);
#3745=SHAPE_DEFINITION_REPRESENTATION(#3772,#3822);
#3746=SHAPE_DEFINITION_REPRESENTATION(#3773,#3823);
#3747=SHAPE_DEFINITION_REPRESENTATION(#3774,#3824);
#3748=SHAPE_DEFINITION_REPRESENTATION(#3775,#3825);
#3749=SHAPE_DEFINITION_REPRESENTATION(#3776,#3826);
#3750=SHAPE_DEFINITION_REPRESENTATION(#3777,#3827);
#3751=SHAPE_DEFINITION_REPRESENTATION(#3778,#3828);
#3752=SHAPE_DEFINITION_REPRESENTATION(#3779,#3829);
#3753=SHAPE_DEFINITION_REPRESENTATION(#3780,#3830);
#3754=SHAPE_DEFINITION_REPRESENTATION(#3781,#3831);
#3755=SHAPE_DEFINITION_REPRESENTATION(#3782,#3832);
#3756=SHAPE_DEFINITION_REPRESENTATION(#3783,#3833);
#3757=PRODUCT_DEFINITION_SHAPE('',$,#3835);
#3758=PRODUCT_DEFINITION_SHAPE('',$,#3836);
#3759=PRODUCT_DEFINITION_SHAPE('',$,#3837);
#3760=PRODUCT_DEFINITION_SHAPE($,$,#104);
#3761=PRODUCT_DEFINITION_SHAPE('',$,#3838);
#3762=PRODUCT_DEFINITION_SHAPE('',$,#3839);
#3763=PRODUCT_DEFINITION_SHAPE('',$,#3840);
#3764=PRODUCT_DEFINITION_SHAPE('',$,#3841);
#3765=PRODUCT_DEFINITION_SHAPE('',$,#3842);
#3766=PRODUCT_DEFINITION_SHAPE('',$,#3843);
#3767=PRODUCT_DEFINITION_SHAPE('',$,#3844);
#3768=PRODUCT_DEFINITION_SHAPE('',$,#3845);
#3769=PRODUCT_DEFINITION_SHAPE('',$,#3846);
#3770=PRODUCT_DEFINITION_SHAPE('',$,#3847);
#3771=PRODUCT_DEFINITION_SHAPE('',$,#3848);
#3772=PRODUCT_DEFINITION_SHAPE('',$,#3849);
#3773=PRODUCT_DEFINITION_SHAPE('',$,#3850);
#3774=PRODUCT_DEFINITION_SHAPE('',$,#3851);
#3775=PRODUCT_DEFINITION_SHAPE('',$,#3852);
#3776=PRODUCT_DEFINITION_SHAPE('',$,#3853);
#3777=PRODUCT_DEFINITION_SHAPE('',$,#3854);
#3778=PRODUCT_DEFINITION_SHAPE('',$,#3855);
#3779=PRODUCT_DEFINITION_SHAPE('',$,#3856);
#3780=PRODUCT_DEFINITION_SHAPE('',$,#3857);
#3781=PRODUCT_DEFINITION_SHAPE('',$,#3858);
#3782=PRODUCT_DEFINITION_SHAPE('',$,#3859);
#3783=PRODUCT_DEFINITION_SHAPE('',$,#3860);
#3784=PRODUCT_DEFINITION_SHAPE($,$,#105);
#3785=PRODUCT_DEFINITION_SHAPE($,$,#106);
#3786=PRODUCT_DEFINITION_SHAPE($,$,#107);
#3787=PRODUCT_DEFINITION_SHAPE($,$,#108);
#3788=PRODUCT_DEFINITION_SHAPE($,$,#109);
#3789=PRODUCT_DEFINITION_SHAPE($,$,#110);
#3790=PRODUCT_DEFINITION_SHAPE($,$,#111);
#3791=PRODUCT_DEFINITION_SHAPE($,$,#112);
#3792=PRODUCT_DEFINITION_SHAPE($,$,#113);
#3793=PRODUCT_DEFINITION_SHAPE($,$,#114);
#3794=PRODUCT_DEFINITION_SHAPE($,$,#115);
#3795=PRODUCT_DEFINITION_SHAPE($,$,#116);
#3796=PRODUCT_DEFINITION_SHAPE($,$,#117);
#3797=PRODUCT_DEFINITION_SHAPE($,$,#118);
#3798=PRODUCT_DEFINITION_SHAPE($,$,#119);
#3799=PRODUCT_DEFINITION_SHAPE($,$,#120);
#3800=PRODUCT_DEFINITION_SHAPE($,$,#121);
#3801=PRODUCT_DEFINITION_SHAPE($,$,#122);
#3802=PRODUCT_DEFINITION_SHAPE($,$,#123);
#3803=PRODUCT_DEFINITION_SHAPE($,$,#124);
#3804=PRODUCT_DEFINITION_SHAPE($,$,#125);
#3805=PRODUCT_DEFINITION_SHAPE($,$,#126);
#3806=PRODUCT_DEFINITION_SHAPE($,$,#127);
#3807=PRODUCT_DEFINITION_SHAPE($,$,#128);
#3808=SHAPE_REPRESENTATION('',(#2314,#2479,#2480,#2481,#2482,#2483,#2484,
#2485,#2486,#2487,#2488,#2489,#2490,#2491,#2492,#2493,#2494,#2495,#2496,
#2497,#2498,#2499,#2500,#2501,#2502),#3697);
#3809=SHAPE_REPRESENTATION('',(#2315,#2323),#3698);
#3810=SHAPE_REPRESENTATION('',(#2316),#3699);
#3811=SHAPE_REPRESENTATION('',(#2324),#3700);
#3812=SHAPE_REPRESENTATION('',(#2331),#3701);
#3813=SHAPE_REPRESENTATION('',(#2338),#3702);
#3814=SHAPE_REPRESENTATION('',(#2345),#3703);
#3815=SHAPE_REPRESENTATION('',(#2351),#3704);
#3816=SHAPE_REPRESENTATION('',(#2358),#3705);
#3817=SHAPE_REPRESENTATION('',(#2365),#3706);
#3818=SHAPE_REPRESENTATION('',(#2372),#3707);
#3819=SHAPE_REPRESENTATION('',(#2379),#3708);
#3820=SHAPE_REPRESENTATION('',(#2386),#3709);
#3821=SHAPE_REPRESENTATION('',(#2393),#3710);
#3822=SHAPE_REPRESENTATION('',(#2399),#3711);
#3823=SHAPE_REPRESENTATION('',(#2406),#3712);
#3824=SHAPE_REPRESENTATION('',(#2413),#3713);
#3825=SHAPE_REPRESENTATION('',(#2420),#3714);
#3826=SHAPE_REPRESENTATION('',(#2427),#3715);
#3827=SHAPE_REPRESENTATION('',(#2434),#3716);
#3828=SHAPE_REPRESENTATION('',(#2440),#3717);
#3829=SHAPE_REPRESENTATION('',(#2446),#3718);
#3830=SHAPE_REPRESENTATION('',(#2452),#3719);
#3831=SHAPE_REPRESENTATION('',(#2458),#3720);
#3832=SHAPE_REPRESENTATION('',(#2465),#3721);
#3833=SHAPE_REPRESENTATION('',(#2472),#3722);
#3834=PRODUCT_DEFINITION_CONTEXT('part definition',#3914,'design');
#3835=PRODUCT_DEFINITION('2026-11-15-23-13-34-846','TAS-018',#3861,#3834);
#3836=PRODUCT_DEFINITION('2026-11-15-23-13-34-847','Wardrobe',#3862,#3834);
#3837=PRODUCT_DEFINITION('2026-11-15-23-13-34-848','Right Side Panel',#3863,
#3834);
#3838=PRODUCT_DEFINITION('2026-11-15-23-13-34-849','Left Side Panel',#3864,
#3834);
#3839=PRODUCT_DEFINITION('2026-11-15-23-13-34-850',
'Center Divider Panel',#3865,#3834);
#3840=PRODUCT_DEFINITION('2026-11-15-23-13-34-851',
'Left Lower Small Shelf',#3866,#3834);
#3841=PRODUCT_DEFINITION('2026-11-15-23-13-34-852','Foot Front Center',
#3867,#3834);
#3842=PRODUCT_DEFINITION('2026-11-15-23-13-34-853','Left Lower Divider',
#3868,#3834);
#3843=PRODUCT_DEFINITION('2026-11-15-23-13-34-854','Right Top Shelf',#3869,
#3834);
#3844=PRODUCT_DEFINITION('2026-11-15-23-13-34-855',
'Left Upper Small Shelf',#3870,#3834);
#3845=PRODUCT_DEFINITION('2026-11-15-23-13-34-856',
'Right Upper Divider',#3871,#3834);
#3846=PRODUCT_DEFINITION('2026-11-15-23-13-34-857','Left Mid Shelf',#3872,
#3834);
#3847=PRODUCT_DEFINITION('2026-11-15-23-13-34-858',
'Right Lower Divider',#3873,#3834);
#3848=PRODUCT_DEFINITION('2026-11-15-23-13-34-859','Foot Front Right',#3874,
#3834);
#3849=PRODUCT_DEFINITION('2026-11-15-23-13-34-860','Right Mid Shelf',#3875,
#3834);
#3850=PRODUCT_DEFINITION('2026-11-15-23-13-34-861','Left Top Shelf',#3876,
#3834);
#3851=PRODUCT_DEFINITION('2026-11-15-23-13-34-862','Right Small Shelf',
#3877,#3834);
#3852=PRODUCT_DEFINITION('2026-11-15-23-13-34-863','Left Upper Divider',
#3878,#3834);
#3853=PRODUCT_DEFINITION('2026-11-15-23-13-34-864','Top Panel',#3879,#3834);
#3854=PRODUCT_DEFINITION('2026-11-15-23-13-34-865','Foot Front Left',#3880,
#3834);
#3855=PRODUCT_DEFINITION('2026-11-15-23-13-34-866','Foot Back Right',#3881,
#3834);
#3856=PRODUCT_DEFINITION('2026-11-15-23-13-34-867','Foot Back Left',#3882,
#3834);
#3857=PRODUCT_DEFINITION('2026-11-15-23-13-34-868','Foot Back Center',#3883,
#3834);
#3858=PRODUCT_DEFINITION('2026-11-15-23-13-34-869','Left Back Panel',#3884,
#3834);
#3859=PRODUCT_DEFINITION('2026-11-15-23-13-34-870','Bottom Panel',#3885,
#3834);
#3860=PRODUCT_DEFINITION('2026-11-15-23-13-34-871','Right Back Panel',#3886,
#3834);
#3861=PRODUCT_DEFINITION_FORMATION('',$,#3916);
#3862=PRODUCT_DEFINITION_FORMATION('',$,#3917);
#3863=PRODUCT_DEFINITION_FORMATION('',$,#3918);
#3864=PRODUCT_DEFINITION_FORMATION('',$,#3919);
#3865=PRODUCT_DEFINITION_FORMATION('',$,#3920);
#3866=PRODUCT_DEFINITION_FORMATION('',$,#3921);
#3867=PRODUCT_DEFINITION_FORMATION('',$,#3922);
#3868=PRODUCT_DEFINITION_FORMATION('',$,#3923);
#3869=PRODUCT_DEFINITION_FORMATION('',$,#3924);
#3870=PRODUCT_DEFINITION_FORMATION('',$,#3925);
#3871=PRODUCT_DEFINITION_FORMATION('',$,#3926);
#3872=PRODUCT_DEFINITION_FORMATION('',$,#3927);
#3873=PRODUCT_DEFINITION_FORMATION('',$,#3928);
#3874=PRODUCT_DEFINITION_FORMATION('',$,#3929);
#3875=PRODUCT_DEFINITION_FORMATION('',$,#3930);
#3876=PRODUCT_DEFINITION_FORMATION('',$,#3931);
#3877=PRODUCT_DEFINITION_FORMATION('',$,#3932);
#3878=PRODUCT_DEFINITION_FORMATION('',$,#3933);
#3879=PRODUCT_DEFINITION_FORMATION('',$,#3934);
#3880=PRODUCT_DEFINITION_FORMATION('',$,#3935);
#3881=PRODUCT_DEFINITION_FORMATION('',$,#3936);
#3882=PRODUCT_DEFINITION_FORMATION('',$,#3937);
#3883=PRODUCT_DEFINITION_FORMATION('',$,#3938);
#3884=PRODUCT_DEFINITION_FORMATION('',$,#3939);
#3885=PRODUCT_DEFINITION_FORMATION('',$,#3940);
#3886=PRODUCT_DEFINITION_FORMATION('',$,#3941);
#3887=PRODUCT_RELATED_PRODUCT_CATEGORY('TAS-018','TAS-018',(#3916));
#3888=PRODUCT_RELATED_PRODUCT_CATEGORY('Wardrobe','Wardrobe',(#3917));
#3889=PRODUCT_RELATED_PRODUCT_CATEGORY('Right Side Panel',
'Right Side Panel',(#3918));
#3890=PRODUCT_RELATED_PRODUCT_CATEGORY('Left Side Panel',
'Left Side Panel',(#3919));
#3891=PRODUCT_RELATED_PRODUCT_CATEGORY('Center Divider Panel',
'Center Divider Panel',(#3920));
#3892=PRODUCT_RELATED_PRODUCT_CATEGORY('Left Lower Small Shelf',
'Left Lower Small Shelf',(#3921));
#3893=PRODUCT_RELATED_PRODUCT_CATEGORY('Foot Front Center',
'Foot Front Center',(#3922));
#3894=PRODUCT_RELATED_PRODUCT_CATEGORY('Left Lower Divider',
'Left Lower Divider',(#3923));
#3895=PRODUCT_RELATED_PRODUCT_CATEGORY('Right Top Shelf',
'Right Top Shelf',(#3924));
#3896=PRODUCT_RELATED_PRODUCT_CATEGORY('Left Upper Small Shelf',
'Left Upper Small Shelf',(#3925));
#3897=PRODUCT_RELATED_PRODUCT_CATEGORY('Right Upper Divider',
'Right Upper Divider',(#3926));
#3898=PRODUCT_RELATED_PRODUCT_CATEGORY('Left Mid Shelf',
'Left Mid Shelf',(#3927));
#3899=PRODUCT_RELATED_PRODUCT_CATEGORY('Right Lower Divider',
'Right Lower Divider',(#3928));
#3900=PRODUCT_RELATED_PRODUCT_CATEGORY('Foot Front Right',
'Foot Front Right',(#3929));
#3901=PRODUCT_RELATED_PRODUCT_CATEGORY('Right Mid Shelf',
'Right Mid Shelf',(#3930));
#3902=PRODUCT_RELATED_PRODUCT_CATEGORY('Left Top Shelf',
'Left Top Shelf',(#3931));
#3903=PRODUCT_RELATED_PRODUCT_CATEGORY('Right Small Shelf',
'Right Small Shelf',(#3932));
#3904=PRODUCT_RELATED_PRODUCT_CATEGORY('Left Upper Divider',
'Left Upper Divider',(#3933));
#3905=PRODUCT_RELATED_PRODUCT_CATEGORY('Top Panel','Top Panel',(#3934));
#3906=PRODUCT_RELATED_PRODUCT_CATEGORY('Foot Front Left',
'Foot Front Left',(#3935));
#3907=PRODUCT_RELATED_PRODUCT_CATEGORY('Foot Back Right',
'Foot Back Right',(#3936));
#3908=PRODUCT_RELATED_PRODUCT_CATEGORY('Foot Back Left',
'Foot Back Left',(#3937));
#3909=PRODUCT_RELATED_PRODUCT_CATEGORY('Foot Back Center',
'Foot Back Center',(#3938));
#3910=PRODUCT_RELATED_PRODUCT_CATEGORY('Left Back Panel',
'Left Back Panel',(#3939));
#3911=PRODUCT_RELATED_PRODUCT_CATEGORY('Bottom Panel','Bottom Panel',(#3940));
#3912=PRODUCT_RELATED_PRODUCT_CATEGORY('Right Back Panel',
'Right Back Panel',(#3941));
#3913=APPLICATION_PROTOCOL_DEFINITION('international standard',
'automotive_design',2009,#3914);
#3914=APPLICATION_CONTEXT(
'Core Data for Automotive Mechanical Design Process');
#3915=PRODUCT_CONTEXT('part definition',#3914,'mechanical');
#3916=PRODUCT('2026-11-15-23-13-34-846','TAS-018',$,(#3915));
#3917=PRODUCT('2026-11-15-23-13-34-847','Wardrobe',$,(#3915));
#3918=PRODUCT('2026-11-15-23-13-34-848','Right Side Panel',$,(#3915));
#3919=PRODUCT('2026-11-15-23-13-34-849','Left Side Panel',$,(#3915));
#3920=PRODUCT('2026-11-15-23-13-34-850','Center Divider Panel',$,(#3915));
#3921=PRODUCT('2026-11-15-23-13-34-851','Left Lower Small Shelf',$,(#3915));
#3922=PRODUCT('2026-11-15-23-13-34-852','Foot Front Center',$,(#3915));
#3923=PRODUCT('2026-11-15-23-13-34-853','Left Lower Divider',$,(#3915));
#3924=PRODUCT('2026-11-15-23-13-34-854','Right Top Shelf',$,(#3915));
#3925=PRODUCT('2026-11-15-23-13-34-855','Left Upper Small Shelf',$,(#3915));
#3926=PRODUCT('2026-11-15-23-13-34-856','Right Upper Divider',$,(#3915));
#3927=PRODUCT('2026-11-15-23-13-34-857','Left Mid Shelf',$,(#3915));
#3928=PRODUCT('2026-11-15-23-13-34-858','Right Lower Divider',$,(#3915));
#3929=PRODUCT('2026-11-15-23-13-34-859','Foot Front Right',$,(#3915));
#3930=PRODUCT('2026-11-15-23-13-34-860','Right Mid Shelf',$,(#3915));
#3931=PRODUCT('2026-11-15-23-13-34-861','Left Top Shelf',$,(#3915));
#3932=PRODUCT('2026-11-15-23-13-34-862','Right Small Shelf',$,(#3915));
#3933=PRODUCT('2026-11-15-23-13-34-863','Left Upper Divider',$,(#3915));
#3934=PRODUCT('2026-11-15-23-13-34-864','Top Panel',$,(#3915));
#3935=PRODUCT('2026-11-15-23-13-34-865','Foot Front Left',$,(#3915));
#3936=PRODUCT('2026-11-15-23-13-34-866','Foot Back Right',$,(#3915));
#3937=PRODUCT('2026-11-15-23-13-34-867','Foot Back Left',$,(#3915));
#3938=PRODUCT('2026-11-15-23-13-34-868','Foot Back Center',$,(#3915));
#3939=PRODUCT('2026-11-15-23-13-34-869','Left Back Panel',$,(#3915));
#3940=PRODUCT('2026-11-15-23-13-34-870','Bottom Panel',$,(#3915));
#3941=PRODUCT('2026-11-15-23-13-34-871','Right Back Panel',$,(#3915));
#3942=PRESENTATION_STYLE_ASSIGNMENT((#3950));
#3943=PRESENTATION_STYLE_ASSIGNMENT((#3951));
#3944=PRESENTATION_STYLE_ASSIGNMENT((#3952));
#3945=PRESENTATION_STYLE_ASSIGNMENT((#3953));
#3946=PRESENTATION_STYLE_ASSIGNMENT((#3954));
#3947=PRESENTATION_STYLE_ASSIGNMENT((#3955));
#3948=PRESENTATION_STYLE_ASSIGNMENT((#3956));
#3949=PRESENTATION_STYLE_ASSIGNMENT((#3957));
#3950=SURFACE_STYLE_USAGE(.BOTH.,#3958);
#3951=SURFACE_STYLE_USAGE(.BOTH.,#3959);
#3952=SURFACE_STYLE_USAGE(.BOTH.,#3960);
#3953=SURFACE_STYLE_USAGE(.BOTH.,#3961);
#3954=SURFACE_STYLE_USAGE(.BOTH.,#3962);
#3955=SURFACE_STYLE_USAGE(.BOTH.,#3963);
#3956=SURFACE_STYLE_USAGE(.BOTH.,#3964);
#3957=SURFACE_STYLE_USAGE(.BOTH.,#3965);
#3958=SURFACE_SIDE_STYLE('',(#3966));
#3959=SURFACE_SIDE_STYLE('',(#3967));
#3960=SURFACE_SIDE_STYLE('',(#3968));
#3961=SURFACE_SIDE_STYLE('',(#3969));
#3962=SURFACE_SIDE_STYLE('',(#3970));
#3963=SURFACE_SIDE_STYLE('',(#3971));
#3964=SURFACE_SIDE_STYLE('',(#3972));
#3965=SURFACE_SIDE_STYLE('',(#3973));
#3966=SURFACE_STYLE_FILL_AREA(#3974);
#3967=SURFACE_STYLE_FILL_AREA(#3975);
#3968=SURFACE_STYLE_FILL_AREA(#3976);
#3969=SURFACE_STYLE_FILL_AREA(#3977);
#3970=SURFACE_STYLE_FILL_AREA(#3978);
#3971=SURFACE_STYLE_FILL_AREA(#3979);
#3972=SURFACE_STYLE_FILL_AREA(#3980);
#3973=SURFACE_STYLE_FILL_AREA(#3981);
#3974=FILL_AREA_STYLE('Steel - Satin',(#3982));
#3975=FILL_AREA_STYLE('Dark Blue',(#3983));
#3976=FILL_AREA_STYLE('Light Gray',(#3984));
#3977=FILL_AREA_STYLE('Black',(#3985));
#3978=FILL_AREA_STYLE('Gray',(#3986));
#3979=FILL_AREA_STYLE('Light Blue',(#3987));
#3980=FILL_AREA_STYLE('Blue',(#3988));
#3981=FILL_AREA_STYLE('Sky Blue',(#3989));
#3982=FILL_AREA_STYLE_COLOUR('Steel - Satin',#3990);
#3983=FILL_AREA_STYLE_COLOUR('Dark Blue',#3991);
#3984=FILL_AREA_STYLE_COLOUR('Light Gray',#3992);
#3985=FILL_AREA_STYLE_COLOUR('Black',#3993);
#3986=FILL_AREA_STYLE_COLOUR('Gray',#3994);
#3987=FILL_AREA_STYLE_COLOUR('Light Blue',#3995);
#3988=FILL_AREA_STYLE_COLOUR('Blue',#3996);
#3989=FILL_AREA_STYLE_COLOUR('Sky Blue',#3997);
#3990=COLOUR_RGB('Steel - Satin',0.627450980392157,0.627450980392157,0.627450980392157);
#3991=COLOUR_RGB('Dark Blue',0.,0.125490196078431,0.376470588235294);
#3992=COLOUR_RGB('Light Gray',0.827450980392157,0.827450980392157,0.827450980392157);
#3993=COLOUR_RGB('Black',0.0784313725490196,0.0784313725490196,0.0784313725490196);
#3994=COLOUR_RGB('Gray',0.501960784313725,0.501960784313725,0.501960784313725);
#3995=COLOUR_RGB('Light Blue',0.67843137254902,0.847058823529412,0.901960784313726);
#3996=COLOUR_RGB('Blue',0.,0.4,0.8);
#3997=COLOUR_RGB('Sky Blue',0.529411764705882,0.807843137254902,0.92156862745098);
ENDSEC;
END-ISO-10303-21;
